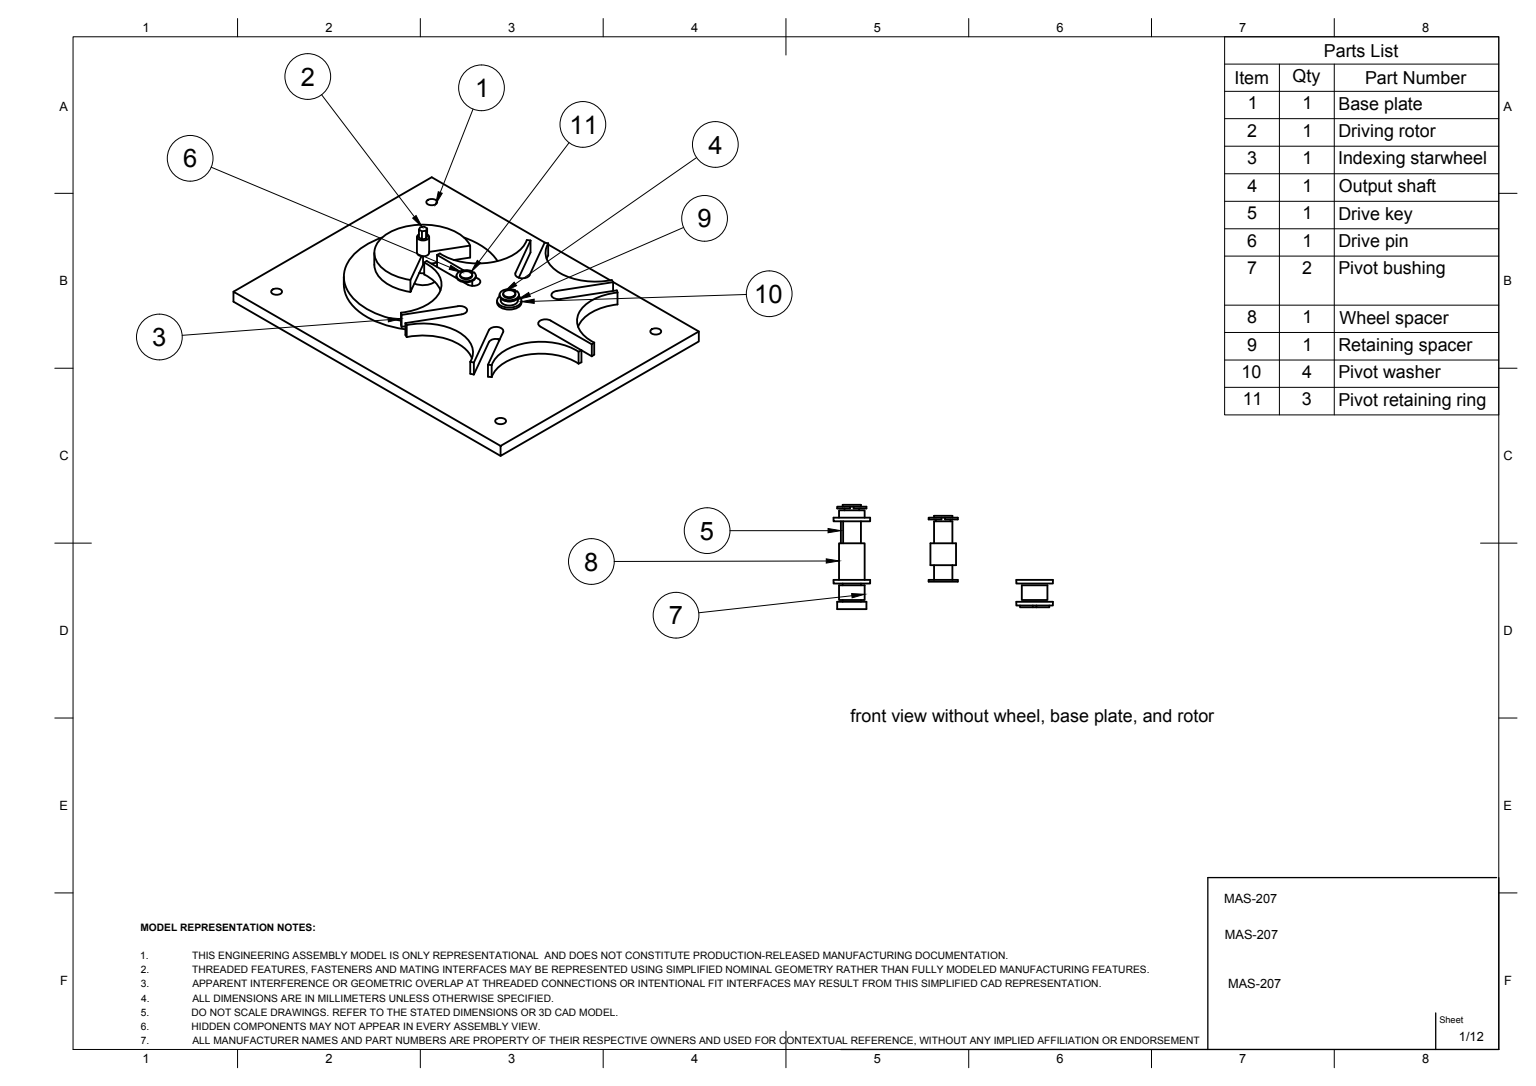
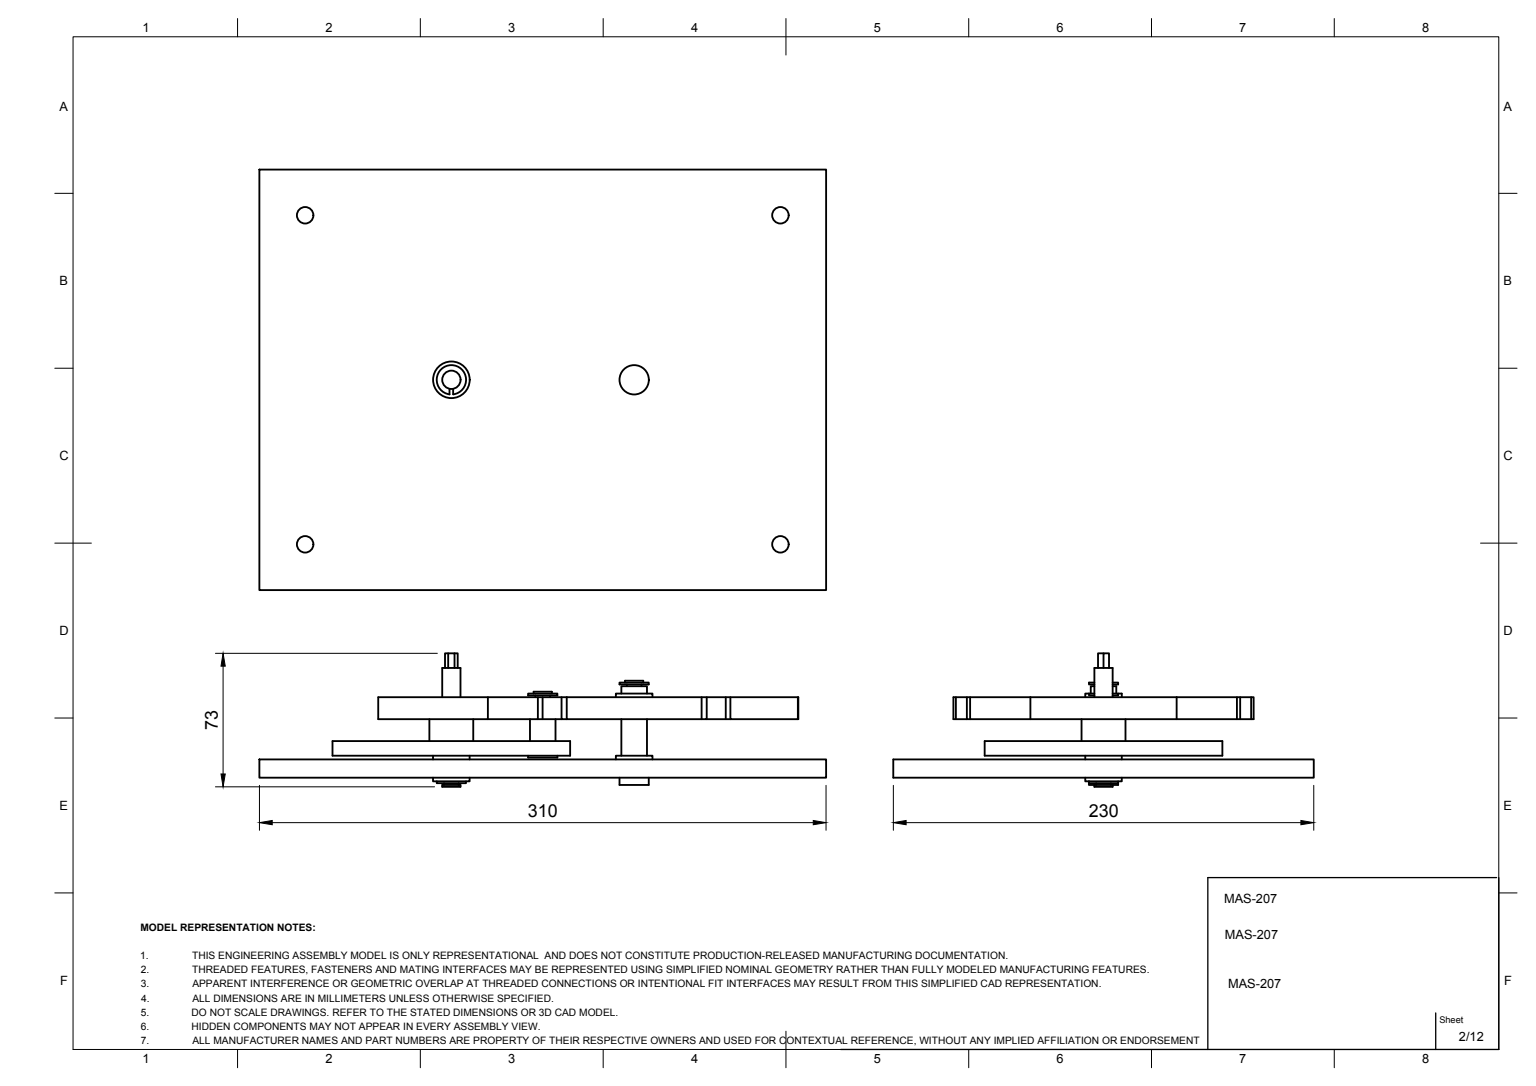
ISO-10303-21;
HEADER;
/* Generated by software containing ST-Developer
 * from STEP Tools, Inc. (www.steptools.com) 
 */

FILE_DESCRIPTION(
/* description */ ('Independent six-slot Geneva indexer. Center distance100, drive radius
50, 60degree indexing per input revolution with120degree engagement an
d240degree dwell. Native machined concave locking faces and relieved d
isk; replaceable retained drive pin; keyed output shaft. Geometry traj
ectory checks use calculated indexing positions, not a contact-dynamic
s simulation. No load or production rating assigned.'),
/* implementation_level */ '2;1');

FILE_NAME(
/* name */ 'MAS-207.step',
/* time_stamp */ '2026-11-09T17:53:22-08:00',
/* author */ (''),
/* organization */ (''),
/* preprocessor_version */ 'ST-DEVELOPER v20.2',
/* originating_system */ 'Autodesk Translation Framework v15.17.0.0',
/* authorisation */ '');

FILE_SCHEMA (('AUTOMOTIVE_DESIGN { 1 0 10303 214 3 1 1 }'));
ENDSEC;

DATA;
#10=MECHANICAL_DESIGN_GEOMETRIC_PRESENTATION_REPRESENTATION('',(#101,#102,
#103,#104,#105,#106,#107,#108,#109,#110,#111),#4149);
#11=ITEM_DEFINED_TRANSFORMATION($,$,#2429,#2700);
#12=ITEM_DEFINED_TRANSFORMATION($,$,#2454,#2701);
#13=ITEM_DEFINED_TRANSFORMATION($,$,#2502,#2702);
#14=ITEM_DEFINED_TRANSFORMATION($,$,#2595,#2703);
#15=ITEM_DEFINED_TRANSFORMATION($,$,#2620,#2704);
#16=ITEM_DEFINED_TRANSFORMATION($,$,#2627,#2705);
#17=ITEM_DEFINED_TRANSFORMATION($,$,#2653,#2706);
#18=ITEM_DEFINED_TRANSFORMATION($,$,#2653,#2707);
#19=ITEM_DEFINED_TRANSFORMATION($,$,#2662,#2708);
#20=ITEM_DEFINED_TRANSFORMATION($,$,#2671,#2709);
#21=ITEM_DEFINED_TRANSFORMATION($,$,#2680,#2710);
#22=ITEM_DEFINED_TRANSFORMATION($,$,#2680,#2711);
#23=ITEM_DEFINED_TRANSFORMATION($,$,#2680,#2712);
#24=ITEM_DEFINED_TRANSFORMATION($,$,#2680,#2713);
#25=ITEM_DEFINED_TRANSFORMATION($,$,#2689,#2714);
#26=ITEM_DEFINED_TRANSFORMATION($,$,#2689,#2715);
#27=ITEM_DEFINED_TRANSFORMATION($,$,#2689,#2716);
#28=(
REPRESENTATION_RELATIONSHIP($,$,#4196,#4195)
REPRESENTATION_RELATIONSHIP_WITH_TRANSFORMATION(#11)
SHAPE_REPRESENTATION_RELATIONSHIP()
);
#29=(
REPRESENTATION_RELATIONSHIP($,$,#4197,#4195)
REPRESENTATION_RELATIONSHIP_WITH_TRANSFORMATION(#12)
SHAPE_REPRESENTATION_RELATIONSHIP()
);
#30=(
REPRESENTATION_RELATIONSHIP($,$,#4198,#4195)
REPRESENTATION_RELATIONSHIP_WITH_TRANSFORMATION(#13)
SHAPE_REPRESENTATION_RELATIONSHIP()
);
#31=(
REPRESENTATION_RELATIONSHIP($,$,#4199,#4195)
REPRESENTATION_RELATIONSHIP_WITH_TRANSFORMATION(#14)
SHAPE_REPRESENTATION_RELATIONSHIP()
);
#32=(
REPRESENTATION_RELATIONSHIP($,$,#4200,#4195)
REPRESENTATION_RELATIONSHIP_WITH_TRANSFORMATION(#15)
SHAPE_REPRESENTATION_RELATIONSHIP()
);
#33=(
REPRESENTATION_RELATIONSHIP($,$,#4201,#4195)
REPRESENTATION_RELATIONSHIP_WITH_TRANSFORMATION(#16)
SHAPE_REPRESENTATION_RELATIONSHIP()
);
#34=(
REPRESENTATION_RELATIONSHIP($,$,#4202,#4195)
REPRESENTATION_RELATIONSHIP_WITH_TRANSFORMATION(#17)
SHAPE_REPRESENTATION_RELATIONSHIP()
);
#35=(
REPRESENTATION_RELATIONSHIP($,$,#4202,#4195)
REPRESENTATION_RELATIONSHIP_WITH_TRANSFORMATION(#18)
SHAPE_REPRESENTATION_RELATIONSHIP()
);
#36=(
REPRESENTATION_RELATIONSHIP($,$,#4203,#4195)
REPRESENTATION_RELATIONSHIP_WITH_TRANSFORMATION(#19)
SHAPE_REPRESENTATION_RELATIONSHIP()
);
#37=(
REPRESENTATION_RELATIONSHIP($,$,#4204,#4195)
REPRESENTATION_RELATIONSHIP_WITH_TRANSFORMATION(#20)
SHAPE_REPRESENTATION_RELATIONSHIP()
);
#38=(
REPRESENTATION_RELATIONSHIP($,$,#4205,#4195)
REPRESENTATION_RELATIONSHIP_WITH_TRANSFORMATION(#21)
SHAPE_REPRESENTATION_RELATIONSHIP()
);
#39=(
REPRESENTATION_RELATIONSHIP($,$,#4205,#4195)
REPRESENTATION_RELATIONSHIP_WITH_TRANSFORMATION(#22)
SHAPE_REPRESENTATION_RELATIONSHIP()
);
#40=(
REPRESENTATION_RELATIONSHIP($,$,#4205,#4195)
REPRESENTATION_RELATIONSHIP_WITH_TRANSFORMATION(#23)
SHAPE_REPRESENTATION_RELATIONSHIP()
);
#41=(
REPRESENTATION_RELATIONSHIP($,$,#4205,#4195)
REPRESENTATION_RELATIONSHIP_WITH_TRANSFORMATION(#24)
SHAPE_REPRESENTATION_RELATIONSHIP()
);
#42=(
REPRESENTATION_RELATIONSHIP($,$,#4206,#4195)
REPRESENTATION_RELATIONSHIP_WITH_TRANSFORMATION(#25)
SHAPE_REPRESENTATION_RELATIONSHIP()
);
#43=(
REPRESENTATION_RELATIONSHIP($,$,#4206,#4195)
REPRESENTATION_RELATIONSHIP_WITH_TRANSFORMATION(#26)
SHAPE_REPRESENTATION_RELATIONSHIP()
);
#44=(
REPRESENTATION_RELATIONSHIP($,$,#4206,#4195)
REPRESENTATION_RELATIONSHIP_WITH_TRANSFORMATION(#27)
SHAPE_REPRESENTATION_RELATIONSHIP()
);
#45=CONTEXT_DEPENDENT_SHAPE_REPRESENTATION(#28,#4178);
#46=CONTEXT_DEPENDENT_SHAPE_REPRESENTATION(#29,#4179);
#47=CONTEXT_DEPENDENT_SHAPE_REPRESENTATION(#30,#4180);
#48=CONTEXT_DEPENDENT_SHAPE_REPRESENTATION(#31,#4181);
#49=CONTEXT_DEPENDENT_SHAPE_REPRESENTATION(#32,#4182);
#50=CONTEXT_DEPENDENT_SHAPE_REPRESENTATION(#33,#4183);
#51=CONTEXT_DEPENDENT_SHAPE_REPRESENTATION(#34,#4184);
#52=CONTEXT_DEPENDENT_SHAPE_REPRESENTATION(#35,#4185);
#53=CONTEXT_DEPENDENT_SHAPE_REPRESENTATION(#36,#4186);
#54=CONTEXT_DEPENDENT_SHAPE_REPRESENTATION(#37,#4187);
#55=CONTEXT_DEPENDENT_SHAPE_REPRESENTATION(#38,#4188);
#56=CONTEXT_DEPENDENT_SHAPE_REPRESENTATION(#39,#4189);
#57=CONTEXT_DEPENDENT_SHAPE_REPRESENTATION(#40,#4190);
#58=CONTEXT_DEPENDENT_SHAPE_REPRESENTATION(#41,#4191);
#59=CONTEXT_DEPENDENT_SHAPE_REPRESENTATION(#42,#4192);
#60=CONTEXT_DEPENDENT_SHAPE_REPRESENTATION(#43,#4193);
#61=CONTEXT_DEPENDENT_SHAPE_REPRESENTATION(#44,#4194);
#62=NEXT_ASSEMBLY_USAGE_OCCURRENCE('Base plate:1','Base plate:1',
'Base plate:1',#4208,#4209,'Base plate:1');
#63=NEXT_ASSEMBLY_USAGE_OCCURRENCE('Driving rotor:1','Driving rotor:1',
'Driving rotor:1',#4208,#4210,'Driving rotor:1');
#64=NEXT_ASSEMBLY_USAGE_OCCURRENCE('Indexing starwheel:1',
'Indexing starwheel:1','Indexing starwheel:1',#4208,#4211,
'Indexing starwheel:1');
#65=NEXT_ASSEMBLY_USAGE_OCCURRENCE('Output shaft:1','Output shaft:1',
'Output shaft:1',#4208,#4212,'Output shaft:1');
#66=NEXT_ASSEMBLY_USAGE_OCCURRENCE('Drive key:1','Drive key:1',
'Drive key:1',#4208,#4213,'Drive key:1');
#67=NEXT_ASSEMBLY_USAGE_OCCURRENCE('Drive pin:1','Drive pin:1',
'Drive pin:1',#4208,#4214,'Drive pin:1');
#68=NEXT_ASSEMBLY_USAGE_OCCURRENCE('Pivot bushing:1','Pivot bushing:1',
'Pivot bushing:1',#4208,#4215,'Pivot bushing:1');
#69=NEXT_ASSEMBLY_USAGE_OCCURRENCE('Pivot bushing:2','Pivot bushing:2',
'Pivot bushing:2',#4208,#4215,'Pivot bushing:2');
#70=NEXT_ASSEMBLY_USAGE_OCCURRENCE('Wheel spacer:1','Wheel spacer:1',
'Wheel spacer:1',#4208,#4216,'Wheel spacer:1');
#71=NEXT_ASSEMBLY_USAGE_OCCURRENCE('Retaining spacer:1',
'Retaining spacer:1','Retaining spacer:1',#4208,#4217,
'Retaining spacer:1');
#72=NEXT_ASSEMBLY_USAGE_OCCURRENCE('Pivot washer:1','Pivot washer:1',
'Pivot washer:1',#4208,#4218,'Pivot washer:1');
#73=NEXT_ASSEMBLY_USAGE_OCCURRENCE('Pivot washer:2','Pivot washer:2',
'Pivot washer:2',#4208,#4218,'Pivot washer:2');
#74=NEXT_ASSEMBLY_USAGE_OCCURRENCE('Pivot washer:3','Pivot washer:3',
'Pivot washer:3',#4208,#4218,'Pivot washer:3');
#75=NEXT_ASSEMBLY_USAGE_OCCURRENCE('Pivot washer:4','Pivot washer:4',
'Pivot washer:4',#4208,#4218,'Pivot washer:4');
#76=NEXT_ASSEMBLY_USAGE_OCCURRENCE('Pivot retaining ring:1',
'Pivot retaining ring:1','Pivot retaining ring:1',#4208,#4219,
'Pivot retaining ring:1');
#77=NEXT_ASSEMBLY_USAGE_OCCURRENCE('Pivot retaining ring:2',
'Pivot retaining ring:2','Pivot retaining ring:2',#4208,#4219,
'Pivot retaining ring:2');
#78=NEXT_ASSEMBLY_USAGE_OCCURRENCE('Pivot retaining ring:3',
'Pivot retaining ring:3','Pivot retaining ring:3',#4208,#4219,
'Pivot retaining ring:3');
#79=SHAPE_REPRESENTATION_RELATIONSHIP('SRR','None',#4196,#90);
#80=SHAPE_REPRESENTATION_RELATIONSHIP('SRR','None',#4197,#91);
#81=SHAPE_REPRESENTATION_RELATIONSHIP('SRR','None',#4198,#92);
#82=SHAPE_REPRESENTATION_RELATIONSHIP('SRR','None',#4199,#93);
#83=SHAPE_REPRESENTATION_RELATIONSHIP('SRR','None',#4200,#94);
#84=SHAPE_REPRESENTATION_RELATIONSHIP('SRR','None',#4201,#95);
#85=SHAPE_REPRESENTATION_RELATIONSHIP('SRR','None',#4202,#96);
#86=SHAPE_REPRESENTATION_RELATIONSHIP('SRR','None',#4203,#97);
#87=SHAPE_REPRESENTATION_RELATIONSHIP('SRR','None',#4204,#98);
#88=SHAPE_REPRESENTATION_RELATIONSHIP('SRR','None',#4205,#99);
#89=SHAPE_REPRESENTATION_RELATIONSHIP('SRR','None',#4206,#100);
#90=ADVANCED_BREP_SHAPE_REPRESENTATION('',(#112),#4138);
#91=ADVANCED_BREP_SHAPE_REPRESENTATION('',(#113),#4139);
#92=ADVANCED_BREP_SHAPE_REPRESENTATION('',(#114),#4140);
#93=ADVANCED_BREP_SHAPE_REPRESENTATION('',(#115),#4141);
#94=ADVANCED_BREP_SHAPE_REPRESENTATION('',(#116),#4142);
#95=ADVANCED_BREP_SHAPE_REPRESENTATION('',(#117),#4143);
#96=ADVANCED_BREP_SHAPE_REPRESENTATION('',(#118),#4144);
#97=ADVANCED_BREP_SHAPE_REPRESENTATION('',(#119),#4145);
#98=ADVANCED_BREP_SHAPE_REPRESENTATION('',(#120),#4146);
#99=ADVANCED_BREP_SHAPE_REPRESENTATION('',(#121),#4147);
#100=ADVANCED_BREP_SHAPE_REPRESENTATION('',(#122),#4148);
#101=STYLED_ITEM('',(#4260),#112);
#102=STYLED_ITEM('',(#4261),#113);
#103=STYLED_ITEM('',(#4262),#114);
#104=STYLED_ITEM('',(#4263),#115);
#105=STYLED_ITEM('',(#4264),#116);
#106=STYLED_ITEM('',(#4263),#117);
#107=STYLED_ITEM('',(#4265),#118);
#108=STYLED_ITEM('',(#4266),#119);
#109=STYLED_ITEM('',(#4266),#120);
#110=STYLED_ITEM('',(#4267),#121);
#111=STYLED_ITEM('',(#4268),#122);
#112=MANIFOLD_SOLID_BREP('Body1',#2295);
#113=MANIFOLD_SOLID_BREP('Body1',#2296);
#114=MANIFOLD_SOLID_BREP('Body1',#2297);
#115=MANIFOLD_SOLID_BREP('Body1',#2298);
#116=MANIFOLD_SOLID_BREP('Body1',#2299);
#117=MANIFOLD_SOLID_BREP('Body1',#2300);
#118=MANIFOLD_SOLID_BREP('Body1',#2301);
#119=MANIFOLD_SOLID_BREP('Body1',#2302);
#120=MANIFOLD_SOLID_BREP('Body1',#2303);
#121=MANIFOLD_SOLID_BREP('Body1',#2304);
#122=MANIFOLD_SOLID_BREP('Body1',#2305);
#123=FACE_BOUND('',#385,.T.);
#124=FACE_BOUND('',#386,.T.);
#125=FACE_BOUND('',#387,.T.);
#126=FACE_BOUND('',#388,.T.);
#127=FACE_BOUND('',#389,.T.);
#128=FACE_BOUND('',#390,.T.);
#129=FACE_BOUND('',#392,.T.);
#130=FACE_BOUND('',#393,.T.);
#131=FACE_BOUND('',#394,.T.);
#132=FACE_BOUND('',#395,.T.);
#133=FACE_BOUND('',#396,.T.);
#134=FACE_BOUND('',#397,.T.);
#135=FACE_BOUND('',#407,.T.);
#136=FACE_BOUND('',#409,.T.);
#137=FACE_BOUND('',#421,.T.);
#138=FACE_BOUND('',#422,.T.);
#139=FACE_BOUND('',#424,.T.);
#140=FACE_BOUND('',#425,.T.);
#141=FACE_BOUND('',#430,.T.);
#142=FACE_BOUND('',#437,.T.);
#143=FACE_BOUND('',#451,.T.);
#144=FACE_BOUND('',#483,.T.);
#145=FACE_BOUND('',#485,.T.);
#146=FACE_BOUND('',#488,.T.);
#147=FACE_BOUND('',#492,.T.);
#148=FACE_BOUND('',#501,.T.);
#149=FACE_BOUND('',#503,.T.);
#150=FACE_BOUND('',#508,.T.);
#151=FACE_BOUND('',#510,.T.);
#152=FACE_BOUND('',#513,.T.);
#153=FACE_BOUND('',#521,.T.);
#154=FACE_BOUND('',#523,.T.);
#155=FACE_BOUND('',#527,.T.);
#156=FACE_BOUND('',#529,.T.);
#157=FACE_BOUND('',#533,.T.);
#158=FACE_BOUND('',#535,.T.);
#159=FACE_BOUND('',#539,.T.);
#160=FACE_BOUND('',#541,.T.);
#161=PLANE('',#2448);
#162=PLANE('',#2449);
#163=PLANE('',#2450);
#164=PLANE('',#2451);
#165=PLANE('',#2452);
#166=PLANE('',#2453);
#167=PLANE('',#2455);
#168=PLANE('',#2456);
#169=PLANE('',#2457);
#170=PLANE('',#2458);
#171=PLANE('',#2459);
#172=PLANE('',#2460);
#173=PLANE('',#2461);
#174=PLANE('',#2465);
#175=PLANE('',#2467);
#176=PLANE('',#2474);
#177=PLANE('',#2476);
#178=PLANE('',#2478);
#179=PLANE('',#2479);
#180=PLANE('',#2480);
#181=PLANE('',#2484);
#182=PLANE('',#2491);
#183=PLANE('',#2493);
#184=PLANE('',#2500);
#185=PLANE('',#2501);
#186=PLANE('',#2503);
#187=PLANE('',#2504);
#188=PLANE('',#2505);
#189=PLANE('',#2509);
#190=PLANE('',#2558);
#191=PLANE('',#2573);
#192=PLANE('',#2574);
#193=PLANE('',#2576);
#194=PLANE('',#2577);
#195=PLANE('',#2579);
#196=PLANE('',#2580);
#197=PLANE('',#2584);
#198=PLANE('',#2585);
#199=PLANE('',#2587);
#200=PLANE('',#2588);
#201=PLANE('',#2592);
#202=PLANE('',#2593);
#203=PLANE('',#2596);
#204=PLANE('',#2597);
#205=PLANE('',#2599);
#206=PLANE('',#2600);
#207=PLANE('',#2601);
#208=PLANE('',#2606);
#209=PLANE('',#2608);
#210=PLANE('',#2612);
#211=PLANE('',#2617);
#212=PLANE('',#2619);
#213=PLANE('',#2621);
#214=PLANE('',#2622);
#215=PLANE('',#2623);
#216=PLANE('',#2624);
#217=PLANE('',#2625);
#218=PLANE('',#2626);
#219=PLANE('',#2628);
#220=PLANE('',#2631);
#221=PLANE('',#2640);
#222=PLANE('',#2642);
#223=PLANE('',#2646);
#224=PLANE('',#2650);
#225=PLANE('',#2652);
#226=PLANE('',#2660);
#227=PLANE('',#2661);
#228=PLANE('',#2669);
#229=PLANE('',#2670);
#230=PLANE('',#2678);
#231=PLANE('',#2679);
#232=PLANE('',#2687);
#233=PLANE('',#2688);
#234=PLANE('',#2690);
#235=PLANE('',#2691);
#236=PLANE('',#2692);
#237=PLANE('',#2699);
#238=FACE_OUTER_BOUND('',#374,.T.);
#239=FACE_OUTER_BOUND('',#375,.T.);
#240=FACE_OUTER_BOUND('',#376,.T.);
#241=FACE_OUTER_BOUND('',#377,.T.);
#242=FACE_OUTER_BOUND('',#378,.T.);
#243=FACE_OUTER_BOUND('',#379,.T.);
#244=FACE_OUTER_BOUND('',#380,.T.);
#245=FACE_OUTER_BOUND('',#381,.T.);
#246=FACE_OUTER_BOUND('',#382,.T.);
#247=FACE_OUTER_BOUND('',#383,.T.);
#248=FACE_OUTER_BOUND('',#384,.T.);
#249=FACE_OUTER_BOUND('',#391,.T.);
#250=FACE_OUTER_BOUND('',#398,.T.);
#251=FACE_OUTER_BOUND('',#399,.T.);
#252=FACE_OUTER_BOUND('',#400,.T.);
#253=FACE_OUTER_BOUND('',#401,.T.);
#254=FACE_OUTER_BOUND('',#402,.T.);
#255=FACE_OUTER_BOUND('',#403,.T.);
#256=FACE_OUTER_BOUND('',#404,.T.);
#257=FACE_OUTER_BOUND('',#405,.T.);
#258=FACE_OUTER_BOUND('',#406,.T.);
#259=FACE_OUTER_BOUND('',#408,.T.);
#260=FACE_OUTER_BOUND('',#410,.T.);
#261=FACE_OUTER_BOUND('',#411,.T.);
#262=FACE_OUTER_BOUND('',#412,.T.);
#263=FACE_OUTER_BOUND('',#413,.T.);
#264=FACE_OUTER_BOUND('',#414,.T.);
#265=FACE_OUTER_BOUND('',#415,.T.);
#266=FACE_OUTER_BOUND('',#416,.T.);
#267=FACE_OUTER_BOUND('',#417,.T.);
#268=FACE_OUTER_BOUND('',#418,.T.);
#269=FACE_OUTER_BOUND('',#419,.T.);
#270=FACE_OUTER_BOUND('',#420,.T.);
#271=FACE_OUTER_BOUND('',#423,.T.);
#272=FACE_OUTER_BOUND('',#426,.T.);
#273=FACE_OUTER_BOUND('',#427,.T.);
#274=FACE_OUTER_BOUND('',#428,.T.);
#275=FACE_OUTER_BOUND('',#429,.T.);
#276=FACE_OUTER_BOUND('',#431,.T.);
#277=FACE_OUTER_BOUND('',#432,.T.);
#278=FACE_OUTER_BOUND('',#433,.T.);
#279=FACE_OUTER_BOUND('',#434,.T.);
#280=FACE_OUTER_BOUND('',#435,.T.);
#281=FACE_OUTER_BOUND('',#436,.T.);
#282=FACE_OUTER_BOUND('',#438,.T.);
#283=FACE_OUTER_BOUND('',#439,.T.);
#284=FACE_OUTER_BOUND('',#440,.T.);
#285=FACE_OUTER_BOUND('',#441,.T.);
#286=FACE_OUTER_BOUND('',#442,.T.);
#287=FACE_OUTER_BOUND('',#443,.T.);
#288=FACE_OUTER_BOUND('',#444,.T.);
#289=FACE_OUTER_BOUND('',#445,.T.);
#290=FACE_OUTER_BOUND('',#446,.T.);
#291=FACE_OUTER_BOUND('',#447,.T.);
#292=FACE_OUTER_BOUND('',#448,.T.);
#293=FACE_OUTER_BOUND('',#449,.T.);
#294=FACE_OUTER_BOUND('',#450,.T.);
#295=FACE_OUTER_BOUND('',#452,.T.);
#296=FACE_OUTER_BOUND('',#453,.T.);
#297=FACE_OUTER_BOUND('',#454,.T.);
#298=FACE_OUTER_BOUND('',#455,.T.);
#299=FACE_OUTER_BOUND('',#456,.T.);
#300=FACE_OUTER_BOUND('',#457,.T.);
#301=FACE_OUTER_BOUND('',#458,.T.);
#302=FACE_OUTER_BOUND('',#459,.T.);
#303=FACE_OUTER_BOUND('',#460,.T.);
#304=FACE_OUTER_BOUND('',#461,.T.);
#305=FACE_OUTER_BOUND('',#462,.T.);
#306=FACE_OUTER_BOUND('',#463,.T.);
#307=FACE_OUTER_BOUND('',#464,.T.);
#308=FACE_OUTER_BOUND('',#465,.T.);
#309=FACE_OUTER_BOUND('',#466,.T.);
#310=FACE_OUTER_BOUND('',#467,.T.);
#311=FACE_OUTER_BOUND('',#468,.T.);
#312=FACE_OUTER_BOUND('',#469,.T.);
#313=FACE_OUTER_BOUND('',#470,.T.);
#314=FACE_OUTER_BOUND('',#471,.T.);
#315=FACE_OUTER_BOUND('',#472,.T.);
#316=FACE_OUTER_BOUND('',#473,.T.);
#317=FACE_OUTER_BOUND('',#474,.T.);
#318=FACE_OUTER_BOUND('',#475,.T.);
#319=FACE_OUTER_BOUND('',#476,.T.);
#320=FACE_OUTER_BOUND('',#477,.T.);
#321=FACE_OUTER_BOUND('',#478,.T.);
#322=FACE_OUTER_BOUND('',#479,.T.);
#323=FACE_OUTER_BOUND('',#480,.T.);
#324=FACE_OUTER_BOUND('',#481,.T.);
#325=FACE_OUTER_BOUND('',#482,.T.);
#326=FACE_OUTER_BOUND('',#484,.T.);
#327=FACE_OUTER_BOUND('',#486,.T.);
#328=FACE_OUTER_BOUND('',#487,.T.);
#329=FACE_OUTER_BOUND('',#489,.T.);
#330=FACE_OUTER_BOUND('',#490,.T.);
#331=FACE_OUTER_BOUND('',#491,.T.);
#332=FACE_OUTER_BOUND('',#493,.T.);
#333=FACE_OUTER_BOUND('',#494,.T.);
#334=FACE_OUTER_BOUND('',#495,.T.);
#335=FACE_OUTER_BOUND('',#496,.T.);
#336=FACE_OUTER_BOUND('',#497,.T.);
#337=FACE_OUTER_BOUND('',#498,.T.);
#338=FACE_OUTER_BOUND('',#499,.T.);
#339=FACE_OUTER_BOUND('',#500,.T.);
#340=FACE_OUTER_BOUND('',#502,.T.);
#341=FACE_OUTER_BOUND('',#504,.T.);
#342=FACE_OUTER_BOUND('',#505,.T.);
#343=FACE_OUTER_BOUND('',#506,.T.);
#344=FACE_OUTER_BOUND('',#507,.T.);
#345=FACE_OUTER_BOUND('',#509,.T.);
#346=FACE_OUTER_BOUND('',#511,.T.);
#347=FACE_OUTER_BOUND('',#512,.T.);
#348=FACE_OUTER_BOUND('',#514,.T.);
#349=FACE_OUTER_BOUND('',#515,.T.);
#350=FACE_OUTER_BOUND('',#516,.T.);
#351=FACE_OUTER_BOUND('',#517,.T.);
#352=FACE_OUTER_BOUND('',#518,.T.);
#353=FACE_OUTER_BOUND('',#519,.T.);
#354=FACE_OUTER_BOUND('',#520,.T.);
#355=FACE_OUTER_BOUND('',#522,.T.);
#356=FACE_OUTER_BOUND('',#524,.T.);
#357=FACE_OUTER_BOUND('',#525,.T.);
#358=FACE_OUTER_BOUND('',#526,.T.);
#359=FACE_OUTER_BOUND('',#528,.T.);
#360=FACE_OUTER_BOUND('',#530,.T.);
#361=FACE_OUTER_BOUND('',#531,.T.);
#362=FACE_OUTER_BOUND('',#532,.T.);
#363=FACE_OUTER_BOUND('',#534,.T.);
#364=FACE_OUTER_BOUND('',#536,.T.);
#365=FACE_OUTER_BOUND('',#537,.T.);
#366=FACE_OUTER_BOUND('',#538,.T.);
#367=FACE_OUTER_BOUND('',#540,.T.);
#368=FACE_OUTER_BOUND('',#542,.T.);
#369=FACE_OUTER_BOUND('',#543,.T.);
#370=FACE_OUTER_BOUND('',#544,.T.);
#371=FACE_OUTER_BOUND('',#545,.T.);
#372=FACE_OUTER_BOUND('',#546,.T.);
#373=FACE_OUTER_BOUND('',#547,.T.);
#374=EDGE_LOOP('',(#1508,#1509,#1510,#1511));
#375=EDGE_LOOP('',(#1512,#1513,#1514,#1515));
#376=EDGE_LOOP('',(#1516,#1517,#1518,#1519));
#377=EDGE_LOOP('',(#1520,#1521,#1522,#1523));
#378=EDGE_LOOP('',(#1524,#1525,#1526,#1527));
#379=EDGE_LOOP('',(#1528,#1529,#1530,#1531));
#380=EDGE_LOOP('',(#1532,#1533,#1534,#1535));
#381=EDGE_LOOP('',(#1536,#1537,#1538,#1539));
#382=EDGE_LOOP('',(#1540,#1541,#1542,#1543));
#383=EDGE_LOOP('',(#1544,#1545,#1546,#1547));
#384=EDGE_LOOP('',(#1548,#1549,#1550,#1551));
#385=EDGE_LOOP('',(#1552));
#386=EDGE_LOOP('',(#1553));
#387=EDGE_LOOP('',(#1554));
#388=EDGE_LOOP('',(#1555));
#389=EDGE_LOOP('',(#1556));
#390=EDGE_LOOP('',(#1557));
#391=EDGE_LOOP('',(#1558,#1559,#1560,#1561));
#392=EDGE_LOOP('',(#1562));
#393=EDGE_LOOP('',(#1563));
#394=EDGE_LOOP('',(#1564));
#395=EDGE_LOOP('',(#1565));
#396=EDGE_LOOP('',(#1566));
#397=EDGE_LOOP('',(#1567));
#398=EDGE_LOOP('',(#1568,#1569,#1570,#1571));
#399=EDGE_LOOP('',(#1572,#1573,#1574,#1575));
#400=EDGE_LOOP('',(#1576,#1577,#1578,#1579));
#401=EDGE_LOOP('',(#1580,#1581,#1582,#1583));
#402=EDGE_LOOP('',(#1584,#1585,#1586,#1587));
#403=EDGE_LOOP('',(#1588,#1589,#1590,#1591));
#404=EDGE_LOOP('',(#1592,#1593,#1594,#1595,#1596,#1597));
#405=EDGE_LOOP('',(#1598,#1599,#1600,#1601));
#406=EDGE_LOOP('',(#1602));
#407=EDGE_LOOP('',(#1603));
#408=EDGE_LOOP('',(#1604));
#409=EDGE_LOOP('',(#1605));
#410=EDGE_LOOP('',(#1606,#1607,#1608,#1609));
#411=EDGE_LOOP('',(#1610,#1611,#1612,#1613));
#412=EDGE_LOOP('',(#1614,#1615,#1616));
#413=EDGE_LOOP('',(#1617,#1618,#1619));
#414=EDGE_LOOP('',(#1620,#1621,#1622,#1623,#1624,#1625));
#415=EDGE_LOOP('',(#1626,#1627,#1628,#1629,#1630,#1631));
#416=EDGE_LOOP('',(#1632,#1633,#1634,#1635,#1636));
#417=EDGE_LOOP('',(#1637,#1638,#1639,#1640,#1641));
#418=EDGE_LOOP('',(#1642,#1643,#1644,#1645));
#419=EDGE_LOOP('',(#1646,#1647,#1648,#1649,#1650,#1651));
#420=EDGE_LOOP('',(#1652));
#421=EDGE_LOOP('',(#1653));
#422=EDGE_LOOP('',(#1654));
#423=EDGE_LOOP('',(#1655));
#424=EDGE_LOOP('',(#1656));
#425=EDGE_LOOP('',(#1657));
#426=EDGE_LOOP('',(#1658,#1659,#1660,#1661));
#427=EDGE_LOOP('',(#1662,#1663,#1664,#1665));
#428=EDGE_LOOP('',(#1666,#1667,#1668,#1669,#1670,#1671));
#429=EDGE_LOOP('',(#1672));
#430=EDGE_LOOP('',(#1673,#1674,#1675,#1676,#1677,#1678));
#431=EDGE_LOOP('',(#1679));
#432=EDGE_LOOP('',(#1680,#1681,#1682,#1683));
#433=EDGE_LOOP('',(#1684,#1685,#1686,#1687));
#434=EDGE_LOOP('',(#1688,#1689,#1690,#1691));
#435=EDGE_LOOP('',(#1692,#1693,#1694,#1695));
#436=EDGE_LOOP('',(#1696,#1697,#1698,#1699,#1700,#1701,#1702,#1703,#1704,
#1705,#1706,#1707,#1708,#1709,#1710,#1711,#1712,#1713,#1714,#1715,#1716,
#1717,#1718,#1719,#1720,#1721,#1722,#1723,#1724,#1725,#1726,#1727,#1728,
#1729,#1730,#1731));
#437=EDGE_LOOP('',(#1732,#1733,#1734,#1735));
#438=EDGE_LOOP('',(#1736,#1737,#1738,#1739));
#439=EDGE_LOOP('',(#1740,#1741,#1742,#1743));
#440=EDGE_LOOP('',(#1744,#1745,#1746,#1747));
#441=EDGE_LOOP('',(#1748,#1749,#1750,#1751));
#442=EDGE_LOOP('',(#1752,#1753,#1754,#1755));
#443=EDGE_LOOP('',(#1756,#1757,#1758,#1759));
#444=EDGE_LOOP('',(#1760,#1761,#1762,#1763));
#445=EDGE_LOOP('',(#1764,#1765,#1766,#1767));
#446=EDGE_LOOP('',(#1768,#1769,#1770,#1771));
#447=EDGE_LOOP('',(#1772,#1773,#1774,#1775));
#448=EDGE_LOOP('',(#1776,#1777,#1778,#1779));
#449=EDGE_LOOP('',(#1780,#1781,#1782,#1783));
#450=EDGE_LOOP('',(#1784,#1785,#1786,#1787,#1788,#1789,#1790,#1791,#1792,
#1793,#1794,#1795,#1796,#1797,#1798,#1799,#1800,#1801,#1802,#1803,#1804,
#1805,#1806,#1807,#1808,#1809,#1810,#1811,#1812,#1813,#1814,#1815,#1816,
#1817,#1818,#1819));
#451=EDGE_LOOP('',(#1820,#1821,#1822,#1823));
#452=EDGE_LOOP('',(#1824,#1825,#1826,#1827));
#453=EDGE_LOOP('',(#1828,#1829,#1830,#1831));
#454=EDGE_LOOP('',(#1832,#1833,#1834,#1835));
#455=EDGE_LOOP('',(#1836,#1837,#1838,#1839));
#456=EDGE_LOOP('',(#1840,#1841,#1842,#1843));
#457=EDGE_LOOP('',(#1844,#1845,#1846,#1847));
#458=EDGE_LOOP('',(#1848,#1849,#1850,#1851));
#459=EDGE_LOOP('',(#1852,#1853,#1854,#1855));
#460=EDGE_LOOP('',(#1856,#1857,#1858,#1859));
#461=EDGE_LOOP('',(#1860,#1861,#1862,#1863));
#462=EDGE_LOOP('',(#1864,#1865,#1866,#1867));
#463=EDGE_LOOP('',(#1868,#1869,#1870,#1871));
#464=EDGE_LOOP('',(#1872,#1873,#1874,#1875));
#465=EDGE_LOOP('',(#1876,#1877,#1878,#1879));
#466=EDGE_LOOP('',(#1880,#1881,#1882,#1883));
#467=EDGE_LOOP('',(#1884,#1885,#1886,#1887));
#468=EDGE_LOOP('',(#1888,#1889,#1890,#1891));
#469=EDGE_LOOP('',(#1892,#1893,#1894,#1895));
#470=EDGE_LOOP('',(#1896,#1897,#1898,#1899));
#471=EDGE_LOOP('',(#1900,#1901,#1902,#1903));
#472=EDGE_LOOP('',(#1904,#1905,#1906,#1907));
#473=EDGE_LOOP('',(#1908,#1909,#1910,#1911));
#474=EDGE_LOOP('',(#1912,#1913,#1914,#1915));
#475=EDGE_LOOP('',(#1916,#1917,#1918,#1919));
#476=EDGE_LOOP('',(#1920,#1921,#1922,#1923));
#477=EDGE_LOOP('',(#1924,#1925,#1926,#1927));
#478=EDGE_LOOP('',(#1928,#1929,#1930,#1931));
#479=EDGE_LOOP('',(#1932,#1933,#1934,#1935));
#480=EDGE_LOOP('',(#1936,#1937,#1938,#1939));
#481=EDGE_LOOP('',(#1940,#1941,#1942,#1943));
#482=EDGE_LOOP('',(#1944));
#483=EDGE_LOOP('',(#1945));
#484=EDGE_LOOP('',(#1946));
#485=EDGE_LOOP('',(#1947));
#486=EDGE_LOOP('',(#1948,#1949,#1950,#1951));
#487=EDGE_LOOP('',(#1952));
#488=EDGE_LOOP('',(#1953));
#489=EDGE_LOOP('',(#1954,#1955,#1956,#1957));
#490=EDGE_LOOP('',(#1958));
#491=EDGE_LOOP('',(#1959,#1960,#1961,#1962));
#492=EDGE_LOOP('',(#1963,#1964,#1965,#1966));
#493=EDGE_LOOP('',(#1967));
#494=EDGE_LOOP('',(#1968,#1969,#1970,#1971));
#495=EDGE_LOOP('',(#1972,#1973,#1974,#1975));
#496=EDGE_LOOP('',(#1976,#1977,#1978,#1979));
#497=EDGE_LOOP('',(#1980,#1981,#1982,#1983));
#498=EDGE_LOOP('',(#1984,#1985,#1986,#1987));
#499=EDGE_LOOP('',(#1988,#1989,#1990,#1991));
#500=EDGE_LOOP('',(#1992));
#501=EDGE_LOOP('',(#1993));
#502=EDGE_LOOP('',(#1994));
#503=EDGE_LOOP('',(#1995));
#504=EDGE_LOOP('',(#1996,#1997,#1998,#1999));
#505=EDGE_LOOP('',(#2000,#2001,#2002,#2003));
#506=EDGE_LOOP('',(#2004,#2005,#2006,#2007));
#507=EDGE_LOOP('',(#2008));
#508=EDGE_LOOP('',(#2009));
#509=EDGE_LOOP('',(#2010));
#510=EDGE_LOOP('',(#2011));
#511=EDGE_LOOP('',(#2012,#2013,#2014,#2015));
#512=EDGE_LOOP('',(#2016));
#513=EDGE_LOOP('',(#2017));
#514=EDGE_LOOP('',(#2018,#2019,#2020,#2021));
#515=EDGE_LOOP('',(#2022));
#516=EDGE_LOOP('',(#2023,#2024,#2025,#2026));
#517=EDGE_LOOP('',(#2027));
#518=EDGE_LOOP('',(#2028,#2029,#2030,#2031));
#519=EDGE_LOOP('',(#2032,#2033,#2034,#2035));
#520=EDGE_LOOP('',(#2036));
#521=EDGE_LOOP('',(#2037));
#522=EDGE_LOOP('',(#2038));
#523=EDGE_LOOP('',(#2039));
#524=EDGE_LOOP('',(#2040,#2041,#2042,#2043));
#525=EDGE_LOOP('',(#2044,#2045,#2046,#2047));
#526=EDGE_LOOP('',(#2048));
#527=EDGE_LOOP('',(#2049));
#528=EDGE_LOOP('',(#2050));
#529=EDGE_LOOP('',(#2051));
#530=EDGE_LOOP('',(#2052,#2053,#2054,#2055));
#531=EDGE_LOOP('',(#2056,#2057,#2058,#2059));
#532=EDGE_LOOP('',(#2060));
#533=EDGE_LOOP('',(#2061));
#534=EDGE_LOOP('',(#2062));
#535=EDGE_LOOP('',(#2063));
#536=EDGE_LOOP('',(#2064,#2065,#2066,#2067));
#537=EDGE_LOOP('',(#2068,#2069,#2070,#2071));
#538=EDGE_LOOP('',(#2072));
#539=EDGE_LOOP('',(#2073));
#540=EDGE_LOOP('',(#2074));
#541=EDGE_LOOP('',(#2075));
#542=EDGE_LOOP('',(#2076,#2077,#2078,#2079));
#543=EDGE_LOOP('',(#2080,#2081,#2082,#2083));
#544=EDGE_LOOP('',(#2084,#2085,#2086,#2087));
#545=EDGE_LOOP('',(#2088,#2089,#2090,#2091));
#546=EDGE_LOOP('',(#2092,#2093,#2094,#2095));
#547=EDGE_LOOP('',(#2096,#2097,#2098,#2099));
#548=LINE('',#3473,#720);
#549=LINE('',#3479,#721);
#550=LINE('',#3485,#722);
#551=LINE('',#3491,#723);
#552=LINE('',#3497,#724);
#553=LINE('',#3503,#725);
#554=LINE('',#3508,#726);
#555=LINE('',#3510,#727);
#556=LINE('',#3512,#728);
#557=LINE('',#3513,#729);
#558=LINE('',#3516,#730);
#559=LINE('',#3518,#731);
#560=LINE('',#3519,#732);
#561=LINE('',#3522,#733);
#562=LINE('',#3524,#734);
#563=LINE('',#3525,#735);
#564=LINE('',#3527,#736);
#565=LINE('',#3528,#737);
#566=LINE('',#3535,#738);
#567=LINE('',#3537,#739);
#568=LINE('',#3539,#740);
#569=LINE('',#3540,#741);
#570=LINE('',#3543,#742);
#571=LINE('',#3545,#743);
#572=LINE('',#3546,#744);
#573=LINE('',#3549,#745);
#574=LINE('',#3551,#746);
#575=LINE('',#3552,#747);
#576=LINE('',#3555,#748);
#577=LINE('',#3557,#749);
#578=LINE('',#3558,#750);
#579=LINE('',#3561,#751);
#580=LINE('',#3563,#752);
#581=LINE('',#3564,#753);
#582=LINE('',#3566,#754);
#583=LINE('',#3567,#755);
#584=LINE('',#3573,#756);
#585=LINE('',#3584,#757);
#586=LINE('',#3589,#758);
#587=LINE('',#3596,#759);
#588=LINE('',#3597,#760);
#589=LINE('',#3603,#761);
#590=LINE('',#3604,#762);
#591=LINE('',#3608,#763);
#592=LINE('',#3609,#764);
#593=LINE('',#3610,#765);
#594=LINE('',#3611,#766);
#595=LINE('',#3615,#767);
#596=LINE('',#3616,#768);
#597=LINE('',#3617,#769);
#598=LINE('',#3631,#770);
#599=LINE('',#3640,#771);
#600=LINE('',#3643,#772);
#601=LINE('',#3648,#773);
#602=LINE('',#3655,#774);
#603=LINE('',#3657,#775);
#604=LINE('',#3659,#776);
#605=LINE('',#3660,#777);
#606=LINE('',#3664,#778);
#607=LINE('',#3666,#779);
#608=LINE('',#3668,#780);
#609=LINE('',#3669,#781);
#610=LINE('',#3671,#782);
#611=LINE('',#3672,#783);
#612=LINE('',#3683,#784);
#613=LINE('',#3687,#785);
#614=LINE('',#3695,#786);
#615=LINE('',#3699,#787);
#616=LINE('',#3707,#788);
#617=LINE('',#3711,#789);
#618=LINE('',#3719,#790);
#619=LINE('',#3723,#791);
#620=LINE('',#3731,#792);
#621=LINE('',#3735,#793);
#622=LINE('',#3743,#794);
#623=LINE('',#3747,#795);
#624=LINE('',#3751,#796);
#625=LINE('',#3753,#797);
#626=LINE('',#3757,#798);
#627=LINE('',#3759,#799);
#628=LINE('',#3763,#800);
#629=LINE('',#3765,#801);
#630=LINE('',#3769,#802);
#631=LINE('',#3771,#803);
#632=LINE('',#3775,#804);
#633=LINE('',#3777,#805);
#634=LINE('',#3781,#806);
#635=LINE('',#3784,#807);
#636=LINE('',#3787,#808);
#637=LINE('',#3792,#809);
#638=LINE('',#3795,#810);
#639=LINE('',#3799,#811);
#640=LINE('',#3803,#812);
#641=LINE('',#3807,#813);
#642=LINE('',#3811,#814);
#643=LINE('',#3815,#815);
#644=LINE('',#3818,#816);
#645=LINE('',#3822,#817);
#646=LINE('',#3825,#818);
#647=LINE('',#3829,#819);
#648=LINE('',#3832,#820);
#649=LINE('',#3836,#821);
#650=LINE('',#3839,#822);
#651=LINE('',#3843,#823);
#652=LINE('',#3848,#824);
#653=LINE('',#3851,#825);
#654=LINE('',#3853,#826);
#655=LINE('',#3855,#827);
#656=LINE('',#3857,#828);
#657=LINE('',#3859,#829);
#658=LINE('',#3862,#830);
#659=LINE('',#3863,#831);
#660=LINE('',#3865,#832);
#661=LINE('',#3868,#833);
#662=LINE('',#3869,#834);
#663=LINE('',#3871,#835);
#664=LINE('',#3876,#836);
#665=LINE('',#3877,#837);
#666=LINE('',#3879,#838);
#667=LINE('',#3882,#839);
#668=LINE('',#3883,#840);
#669=LINE('',#3885,#841);
#670=LINE('',#3890,#842);
#671=LINE('',#3892,#843);
#672=LINE('',#3898,#844);
#673=LINE('',#3900,#845);
#674=LINE('',#3902,#846);
#675=LINE('',#3903,#847);
#676=LINE('',#3908,#848);
#677=LINE('',#3909,#849);
#678=LINE('',#3912,#850);
#679=LINE('',#3914,#851);
#680=LINE('',#3915,#852);
#681=LINE('',#3917,#853);
#682=LINE('',#3924,#854);
#683=LINE('',#3935,#855);
#684=LINE('',#3943,#856);
#685=LINE('',#3947,#857);
#686=LINE('',#3953,#858);
#687=LINE('',#3955,#859);
#688=LINE('',#3957,#860);
#689=LINE('',#3958,#861);
#690=LINE('',#3961,#862);
#691=LINE('',#3963,#863);
#692=LINE('',#3964,#864);
#693=LINE('',#3967,#865);
#694=LINE('',#3969,#866);
#695=LINE('',#3970,#867);
#696=LINE('',#3972,#868);
#697=LINE('',#3973,#869);
#698=LINE('',#3988,#870);
#699=LINE('',#3991,#871);
#700=LINE('',#3997,#872);
#701=LINE('',#4008,#873);
#702=LINE('',#4014,#874);
#703=LINE('',#4018,#875);
#704=LINE('',#4025,#876);
#705=LINE('',#4031,#877);
#706=LINE('',#4040,#878);
#707=LINE('',#4046,#879);
#708=LINE('',#4055,#880);
#709=LINE('',#4061,#881);
#710=LINE('',#4070,#882);
#711=LINE('',#4076,#883);
#712=LINE('',#4084,#884);
#713=LINE('',#4086,#885);
#714=LINE('',#4088,#886);
#715=LINE('',#4089,#887);
#716=LINE('',#4093,#888);
#717=LINE('',#4095,#889);
#718=LINE('',#4097,#890);
#719=LINE('',#4098,#891);
#720=VECTOR('',#2725,4.5);
#721=VECTOR('',#2732,4.5);
#722=VECTOR('',#2739,4.5);
#723=VECTOR('',#2746,4.5);
#724=VECTOR('',#2753,7.);
#725=VECTOR('',#2760,7.);
#726=VECTOR('',#2765,10.);
#727=VECTOR('',#2766,10.);
#728=VECTOR('',#2767,10.);
#729=VECTOR('',#2768,10.);
#730=VECTOR('',#2771,10.);
#731=VECTOR('',#2772,10.);
#732=VECTOR('',#2773,10.);
#733=VECTOR('',#2776,10.);
#734=VECTOR('',#2777,10.);
#735=VECTOR('',#2778,10.);
#736=VECTOR('',#2781,10.);
#737=VECTOR('',#2782,10.);
#738=VECTOR('',#2791,10.);
#739=VECTOR('',#2792,10.);
#740=VECTOR('',#2793,10.);
#741=VECTOR('',#2794,10.);
#742=VECTOR('',#2797,10.);
#743=VECTOR('',#2798,10.);
#744=VECTOR('',#2799,10.);
#745=VECTOR('',#2802,10.);
#746=VECTOR('',#2803,10.);
#747=VECTOR('',#2804,10.);
#748=VECTOR('',#2807,10.);
#749=VECTOR('',#2808,10.);
#750=VECTOR('',#2809,10.);
#751=VECTOR('',#2812,10.);
#752=VECTOR('',#2813,10.);
#753=VECTOR('',#2814,10.);
#754=VECTOR('',#2817,10.);
#755=VECTOR('',#2818,10.);
#756=VECTOR('',#2825,4.);
#757=VECTOR('',#2840,5.);
#758=VECTOR('',#2845,5.);
#759=VECTOR('',#2852,10.);
#760=VECTOR('',#2853,10.);
#761=VECTOR('',#2858,10.);
#762=VECTOR('',#2859,10.);
#763=VECTOR('',#2862,10.);
#764=VECTOR('',#2863,10.);
#765=VECTOR('',#2864,10.);
#766=VECTOR('',#2865,10.);
#767=VECTOR('',#2868,10.);
#768=VECTOR('',#2869,10.);
#769=VECTOR('',#2870,10.);
#770=VECTOR('',#2891,12.);
#771=VECTOR('',#2904,60.);
#772=VECTOR('',#2907,5.);
#773=VECTOR('',#2914,5.);
#774=VECTOR('',#2923,10.);
#775=VECTOR('',#2924,10.);
#776=VECTOR('',#2925,10.);
#777=VECTOR('',#2926,10.);
#778=VECTOR('',#2929,10.);
#779=VECTOR('',#2930,10.);
#780=VECTOR('',#2931,10.);
#781=VECTOR('',#2932,10.);
#782=VECTOR('',#2935,10.);
#783=VECTOR('',#2936,10.);
#784=VECTOR('',#2949,10.);
#785=VECTOR('',#2952,10.);
#786=VECTOR('',#2959,10.);
#787=VECTOR('',#2962,10.);
#788=VECTOR('',#2969,10.);
#789=VECTOR('',#2972,10.);
#790=VECTOR('',#2979,10.);
#791=VECTOR('',#2982,10.);
#792=VECTOR('',#2989,10.);
#793=VECTOR('',#2992,10.);
#794=VECTOR('',#2999,10.);
#795=VECTOR('',#3002,10.);
#796=VECTOR('',#3007,10.);
#797=VECTOR('',#3008,10.);
#798=VECTOR('',#3013,10.);
#799=VECTOR('',#3014,10.);
#800=VECTOR('',#3019,10.);
#801=VECTOR('',#3020,10.);
#802=VECTOR('',#3025,10.);
#803=VECTOR('',#3026,10.);
#804=VECTOR('',#3031,10.);
#805=VECTOR('',#3032,10.);
#806=VECTOR('',#3037,10.);
#807=VECTOR('',#3040,10.);
#808=VECTOR('',#3043,10.);
#809=VECTOR('',#3050,10.);
#810=VECTOR('',#3053,10.);
#811=VECTOR('',#3058,10.);
#812=VECTOR('',#3063,10.);
#813=VECTOR('',#3068,10.);
#814=VECTOR('',#3073,10.);
#815=VECTOR('',#3076,10.);
#816=VECTOR('',#3079,10.);
#817=VECTOR('',#3082,10.);
#818=VECTOR('',#3085,10.);
#819=VECTOR('',#3088,10.);
#820=VECTOR('',#3091,10.);
#821=VECTOR('',#3094,10.);
#822=VECTOR('',#3097,10.);
#823=VECTOR('',#3100,10.);
#824=VECTOR('',#3105,10.);
#825=VECTOR('',#3108,10.);
#826=VECTOR('',#3111,10.);
#827=VECTOR('',#3114,10.);
#828=VECTOR('',#3117,10.);
#829=VECTOR('',#3120,10.);
#830=VECTOR('',#3125,10.);
#831=VECTOR('',#3126,10.);
#832=VECTOR('',#3129,10.);
#833=VECTOR('',#3134,10.);
#834=VECTOR('',#3135,10.);
#835=VECTOR('',#3138,10.);
#836=VECTOR('',#3147,10.);
#837=VECTOR('',#3148,10.);
#838=VECTOR('',#3151,10.);
#839=VECTOR('',#3156,10.);
#840=VECTOR('',#3157,10.);
#841=VECTOR('',#3160,10.);
#842=VECTOR('',#3169,10.);
#843=VECTOR('',#3172,10.);
#844=VECTOR('',#3179,10.);
#845=VECTOR('',#3180,10.);
#846=VECTOR('',#3181,10.);
#847=VECTOR('',#3182,10.);
#848=VECTOR('',#3187,10.);
#849=VECTOR('',#3188,10.);
#850=VECTOR('',#3191,10.);
#851=VECTOR('',#3192,10.);
#852=VECTOR('',#3193,10.);
#853=VECTOR('',#3196,10.);
#854=VECTOR('',#3205,4.);
#855=VECTOR('',#3220,5.);
#856=VECTOR('',#3229,8.);
#857=VECTOR('',#3236,5.);
#858=VECTOR('',#3243,10.);
#859=VECTOR('',#3244,10.);
#860=VECTOR('',#3245,10.);
#861=VECTOR('',#3246,10.);
#862=VECTOR('',#3249,10.);
#863=VECTOR('',#3250,10.);
#864=VECTOR('',#3251,10.);
#865=VECTOR('',#3254,10.);
#866=VECTOR('',#3255,10.);
#867=VECTOR('',#3256,10.);
#868=VECTOR('',#3259,10.);
#869=VECTOR('',#3260,10.);
#870=VECTOR('',#3281,7.);
#871=VECTOR('',#3284,5.);
#872=VECTOR('',#3291,4.);
#873=VECTOR('',#3306,5.);
#874=VECTOR('',#3313,8.);
#875=VECTOR('',#3320,5.);
#876=VECTOR('',#3329,5.);
#877=VECTOR('',#3336,7.);
#878=VECTOR('',#3349,5.);
#879=VECTOR('',#3356,7.);
#880=VECTOR('',#3369,5.);
#881=VECTOR('',#3376,7.);
#882=VECTOR('',#3389,5.);
#883=VECTOR('',#3396,10.);
#884=VECTOR('',#3407,10.);
#885=VECTOR('',#3408,10.);
#886=VECTOR('',#3409,10.);
#887=VECTOR('',#3410,10.);
#888=VECTOR('',#3413,10.);
#889=VECTOR('',#3414,10.);
#890=VECTOR('',#3415,10.);
#891=VECTOR('',#3416,10.);
#892=CIRCLE('',#2431,4.5);
#893=CIRCLE('',#2432,4.5);
#894=CIRCLE('',#2434,4.5);
#895=CIRCLE('',#2435,4.5);
#896=CIRCLE('',#2437,4.5);
#897=CIRCLE('',#2438,4.5);
#898=CIRCLE('',#2440,4.5);
#899=CIRCLE('',#2441,4.5);
#900=CIRCLE('',#2443,7.);
#901=CIRCLE('',#2444,7.);
#902=CIRCLE('',#2446,7.);
#903=CIRCLE('',#2447,7.);
#904=CIRCLE('',#2463,4.);
#905=CIRCLE('',#2464,4.);
#906=CIRCLE('',#2466,5.);
#907=CIRCLE('',#2468,5.);
#908=CIRCLE('',#2470,5.);
#909=CIRCLE('',#2472,5.);
#910=CIRCLE('',#2473,5.);
#911=CIRCLE('',#2475,5.);
#912=CIRCLE('',#2477,12.);
#913=CIRCLE('',#2481,5.);
#914=CIRCLE('',#2482,5.);
#915=CIRCLE('',#2483,40.);
#916=CIRCLE('',#2485,40.);
#917=CIRCLE('',#2486,12.);
#918=CIRCLE('',#2487,12.);
#919=CIRCLE('',#2490,12.);
#920=CIRCLE('',#2492,65.);
#921=CIRCLE('',#2494,65.);
#922=CIRCLE('',#2497,5.);
#923=CIRCLE('',#2499,5.);
#924=CIRCLE('',#2507,5.);
#925=CIRCLE('',#2508,5.);
#926=CIRCLE('',#2510,41.);
#927=CIRCLE('',#2511,90.);
#928=CIRCLE('',#2512,6.);
#929=CIRCLE('',#2513,90.);
#930=CIRCLE('',#2514,41.);
#931=CIRCLE('',#2515,90.);
#932=CIRCLE('',#2516,6.);
#933=CIRCLE('',#2517,90.);
#934=CIRCLE('',#2518,41.);
#935=CIRCLE('',#2519,90.);
#936=CIRCLE('',#2520,6.);
#937=CIRCLE('',#2521,90.);
#938=CIRCLE('',#2522,41.);
#939=CIRCLE('',#2523,90.);
#940=CIRCLE('',#2524,6.);
#941=CIRCLE('',#2525,90.);
#942=CIRCLE('',#2526,41.);
#943=CIRCLE('',#2527,90.);
#944=CIRCLE('',#2528,6.);
#945=CIRCLE('',#2529,90.);
#946=CIRCLE('',#2530,41.);
#947=CIRCLE('',#2531,90.);
#948=CIRCLE('',#2532,6.);
#949=CIRCLE('',#2533,90.);
#950=CIRCLE('',#2535,41.);
#951=CIRCLE('',#2537,41.);
#952=CIRCLE('',#2539,41.);
#953=CIRCLE('',#2541,41.);
#954=CIRCLE('',#2543,41.);
#955=CIRCLE('',#2545,41.);
#956=CIRCLE('',#2547,90.);
#957=CIRCLE('',#2549,90.);
#958=CIRCLE('',#2551,90.);
#959=CIRCLE('',#2553,90.);
#960=CIRCLE('',#2555,90.);
#961=CIRCLE('',#2557,90.);
#962=CIRCLE('',#2559,6.);
#963=CIRCLE('',#2560,90.);
#964=CIRCLE('',#2561,6.);
#965=CIRCLE('',#2562,90.);
#966=CIRCLE('',#2563,6.);
#967=CIRCLE('',#2564,90.);
#968=CIRCLE('',#2565,6.);
#969=CIRCLE('',#2566,90.);
#970=CIRCLE('',#2567,6.);
#971=CIRCLE('',#2568,90.);
#972=CIRCLE('',#2569,90.);
#973=CIRCLE('',#2570,6.);
#974=CIRCLE('',#2598,5.);
#975=CIRCLE('',#2602,5.);
#976=CIRCLE('',#2604,4.);
#977=CIRCLE('',#2605,4.);
#978=CIRCLE('',#2607,5.);
#979=CIRCLE('',#2609,5.);
#980=CIRCLE('',#2611,5.);
#981=CIRCLE('',#2613,8.);
#982=CIRCLE('',#2614,5.);
#983=CIRCLE('',#2616,8.);
#984=CIRCLE('',#2629,7.);
#985=CIRCLE('',#2630,5.);
#986=CIRCLE('',#2632,7.);
#987=CIRCLE('',#2633,5.);
#988=CIRCLE('',#2636,5.);
#989=CIRCLE('',#2638,4.);
#990=CIRCLE('',#2639,4.);
#991=CIRCLE('',#2641,5.);
#992=CIRCLE('',#2643,5.);
#993=CIRCLE('',#2645,5.);
#994=CIRCLE('',#2647,8.);
#995=CIRCLE('',#2649,8.);
#996=CIRCLE('',#2655,5.);
#997=CIRCLE('',#2656,5.);
#998=CIRCLE('',#2658,7.);
#999=CIRCLE('',#2659,7.);
#1000=CIRCLE('',#2664,5.);
#1001=CIRCLE('',#2665,5.);
#1002=CIRCLE('',#2667,7.);
#1003=CIRCLE('',#2668,7.);
#1004=CIRCLE('',#2673,5.);
#1005=CIRCLE('',#2674,5.);
#1006=CIRCLE('',#2676,7.);
#1007=CIRCLE('',#2677,7.);
#1008=CIRCLE('',#2682,5.);
#1009=CIRCLE('',#2683,5.);
#1010=CIRCLE('',#2685,10.);
#1011=CIRCLE('',#2686,10.);
#1012=CIRCLE('',#2693,8.);
#1013=CIRCLE('',#2694,4.);
#1014=CIRCLE('',#2696,4.);
#1015=CIRCLE('',#2698,8.);
#1016=VERTEX_POINT('',#3470);
#1017=VERTEX_POINT('',#3472);
#1018=VERTEX_POINT('',#3476);
#1019=VERTEX_POINT('',#3478);
#1020=VERTEX_POINT('',#3482);
#1021=VERTEX_POINT('',#3484);
#1022=VERTEX_POINT('',#3488);
#1023=VERTEX_POINT('',#3490);
#1024=VERTEX_POINT('',#3494);
#1025=VERTEX_POINT('',#3496);
#1026=VERTEX_POINT('',#3500);
#1027=VERTEX_POINT('',#3502);
#1028=VERTEX_POINT('',#3506);
#1029=VERTEX_POINT('',#3507);
#1030=VERTEX_POINT('',#3509);
#1031=VERTEX_POINT('',#3511);
#1032=VERTEX_POINT('',#3515);
#1033=VERTEX_POINT('',#3517);
#1034=VERTEX_POINT('',#3521);
#1035=VERTEX_POINT('',#3523);
#1036=VERTEX_POINT('',#3533);
#1037=VERTEX_POINT('',#3534);
#1038=VERTEX_POINT('',#3536);
#1039=VERTEX_POINT('',#3538);
#1040=VERTEX_POINT('',#3542);
#1041=VERTEX_POINT('',#3544);
#1042=VERTEX_POINT('',#3548);
#1043=VERTEX_POINT('',#3550);
#1044=VERTEX_POINT('',#3554);
#1045=VERTEX_POINT('',#3556);
#1046=VERTEX_POINT('',#3560);
#1047=VERTEX_POINT('',#3562);
#1048=VERTEX_POINT('',#3570);
#1049=VERTEX_POINT('',#3572);
#1050=VERTEX_POINT('',#3576);
#1051=VERTEX_POINT('',#3579);
#1052=VERTEX_POINT('',#3582);
#1053=VERTEX_POINT('',#3586);
#1054=VERTEX_POINT('',#3588);
#1055=VERTEX_POINT('',#3592);
#1056=VERTEX_POINT('',#3593);
#1057=VERTEX_POINT('',#3595);
#1058=VERTEX_POINT('',#3599);
#1059=VERTEX_POINT('',#3600);
#1060=VERTEX_POINT('',#3602);
#1061=VERTEX_POINT('',#3606);
#1062=VERTEX_POINT('',#3607);
#1063=VERTEX_POINT('',#3613);
#1064=VERTEX_POINT('',#3614);
#1065=VERTEX_POINT('',#3619);
#1066=VERTEX_POINT('',#3625);
#1067=VERTEX_POINT('',#3630);
#1068=VERTEX_POINT('',#3634);
#1069=VERTEX_POINT('',#3637);
#1070=VERTEX_POINT('',#3642);
#1071=VERTEX_POINT('',#3646);
#1072=VERTEX_POINT('',#3653);
#1073=VERTEX_POINT('',#3654);
#1074=VERTEX_POINT('',#3656);
#1075=VERTEX_POINT('',#3658);
#1076=VERTEX_POINT('',#3662);
#1077=VERTEX_POINT('',#3663);
#1078=VERTEX_POINT('',#3665);
#1079=VERTEX_POINT('',#3667);
#1080=VERTEX_POINT('',#3677);
#1081=VERTEX_POINT('',#3678);
#1082=VERTEX_POINT('',#3680);
#1083=VERTEX_POINT('',#3682);
#1084=VERTEX_POINT('',#3684);
#1085=VERTEX_POINT('',#3686);
#1086=VERTEX_POINT('',#3688);
#1087=VERTEX_POINT('',#3690);
#1088=VERTEX_POINT('',#3692);
#1089=VERTEX_POINT('',#3694);
#1090=VERTEX_POINT('',#3696);
#1091=VERTEX_POINT('',#3698);
#1092=VERTEX_POINT('',#3700);
#1093=VERTEX_POINT('',#3702);
#1094=VERTEX_POINT('',#3704);
#1095=VERTEX_POINT('',#3706);
#1096=VERTEX_POINT('',#3708);
#1097=VERTEX_POINT('',#3710);
#1098=VERTEX_POINT('',#3712);
#1099=VERTEX_POINT('',#3714);
#1100=VERTEX_POINT('',#3716);
#1101=VERTEX_POINT('',#3718);
#1102=VERTEX_POINT('',#3720);
#1103=VERTEX_POINT('',#3722);
#1104=VERTEX_POINT('',#3724);
#1105=VERTEX_POINT('',#3726);
#1106=VERTEX_POINT('',#3728);
#1107=VERTEX_POINT('',#3730);
#1108=VERTEX_POINT('',#3732);
#1109=VERTEX_POINT('',#3734);
#1110=VERTEX_POINT('',#3736);
#1111=VERTEX_POINT('',#3738);
#1112=VERTEX_POINT('',#3740);
#1113=VERTEX_POINT('',#3742);
#1114=VERTEX_POINT('',#3744);
#1115=VERTEX_POINT('',#3746);
#1116=VERTEX_POINT('',#3750);
#1117=VERTEX_POINT('',#3752);
#1118=VERTEX_POINT('',#3756);
#1119=VERTEX_POINT('',#3758);
#1120=VERTEX_POINT('',#3762);
#1121=VERTEX_POINT('',#3764);
#1122=VERTEX_POINT('',#3768);
#1123=VERTEX_POINT('',#3770);
#1124=VERTEX_POINT('',#3774);
#1125=VERTEX_POINT('',#3776);
#1126=VERTEX_POINT('',#3780);
#1127=VERTEX_POINT('',#3782);
#1128=VERTEX_POINT('',#3786);
#1129=VERTEX_POINT('',#3790);
#1130=VERTEX_POINT('',#3794);
#1131=VERTEX_POINT('',#3798);
#1132=VERTEX_POINT('',#3802);
#1133=VERTEX_POINT('',#3806);
#1134=VERTEX_POINT('',#3810);
#1135=VERTEX_POINT('',#3812);
#1136=VERTEX_POINT('',#3814);
#1137=VERTEX_POINT('',#3817);
#1138=VERTEX_POINT('',#3819);
#1139=VERTEX_POINT('',#3821);
#1140=VERTEX_POINT('',#3824);
#1141=VERTEX_POINT('',#3826);
#1142=VERTEX_POINT('',#3828);
#1143=VERTEX_POINT('',#3831);
#1144=VERTEX_POINT('',#3833);
#1145=VERTEX_POINT('',#3835);
#1146=VERTEX_POINT('',#3838);
#1147=VERTEX_POINT('',#3840);
#1148=VERTEX_POINT('',#3842);
#1149=VERTEX_POINT('',#3845);
#1150=VERTEX_POINT('',#3847);
#1151=VERTEX_POINT('',#3849);
#1152=VERTEX_POINT('',#3896);
#1153=VERTEX_POINT('',#3897);
#1154=VERTEX_POINT('',#3899);
#1155=VERTEX_POINT('',#3901);
#1156=VERTEX_POINT('',#3905);
#1157=VERTEX_POINT('',#3907);
#1158=VERTEX_POINT('',#3911);
#1159=VERTEX_POINT('',#3913);
#1160=VERTEX_POINT('',#3921);
#1161=VERTEX_POINT('',#3923);
#1162=VERTEX_POINT('',#3927);
#1163=VERTEX_POINT('',#3930);
#1164=VERTEX_POINT('',#3933);
#1165=VERTEX_POINT('',#3937);
#1166=VERTEX_POINT('',#3939);
#1167=VERTEX_POINT('',#3942);
#1168=VERTEX_POINT('',#3951);
#1169=VERTEX_POINT('',#3952);
#1170=VERTEX_POINT('',#3954);
#1171=VERTEX_POINT('',#3956);
#1172=VERTEX_POINT('',#3960);
#1173=VERTEX_POINT('',#3962);
#1174=VERTEX_POINT('',#3966);
#1175=VERTEX_POINT('',#3968);
#1176=VERTEX_POINT('',#3978);
#1177=VERTEX_POINT('',#3980);
#1178=VERTEX_POINT('',#3983);
#1179=VERTEX_POINT('',#3985);
#1180=VERTEX_POINT('',#3990);
#1181=VERTEX_POINT('',#3994);
#1182=VERTEX_POINT('',#3996);
#1183=VERTEX_POINT('',#4000);
#1184=VERTEX_POINT('',#4003);
#1185=VERTEX_POINT('',#4006);
#1186=VERTEX_POINT('',#4010);
#1187=VERTEX_POINT('',#4013);
#1188=VERTEX_POINT('',#4022);
#1189=VERTEX_POINT('',#4024);
#1190=VERTEX_POINT('',#4028);
#1191=VERTEX_POINT('',#4030);
#1192=VERTEX_POINT('',#4037);
#1193=VERTEX_POINT('',#4039);
#1194=VERTEX_POINT('',#4043);
#1195=VERTEX_POINT('',#4045);
#1196=VERTEX_POINT('',#4052);
#1197=VERTEX_POINT('',#4054);
#1198=VERTEX_POINT('',#4058);
#1199=VERTEX_POINT('',#4060);
#1200=VERTEX_POINT('',#4067);
#1201=VERTEX_POINT('',#4069);
#1202=VERTEX_POINT('',#4073);
#1203=VERTEX_POINT('',#4075);
#1204=VERTEX_POINT('',#4082);
#1205=VERTEX_POINT('',#4083);
#1206=VERTEX_POINT('',#4085);
#1207=VERTEX_POINT('',#4087);
#1208=VERTEX_POINT('',#4091);
#1209=VERTEX_POINT('',#4092);
#1210=VERTEX_POINT('',#4094);
#1211=VERTEX_POINT('',#4096);
#1212=EDGE_CURVE('',#1016,#1016,#892,.T.);
#1213=EDGE_CURVE('',#1016,#1017,#548,.T.);
#1214=EDGE_CURVE('',#1017,#1017,#893,.T.);
#1215=EDGE_CURVE('',#1018,#1018,#894,.T.);
#1216=EDGE_CURVE('',#1018,#1019,#549,.T.);
#1217=EDGE_CURVE('',#1019,#1019,#895,.T.);
#1218=EDGE_CURVE('',#1020,#1020,#896,.T.);
#1219=EDGE_CURVE('',#1020,#1021,#550,.T.);
#1220=EDGE_CURVE('',#1021,#1021,#897,.T.);
#1221=EDGE_CURVE('',#1022,#1022,#898,.T.);
#1222=EDGE_CURVE('',#1022,#1023,#551,.T.);
#1223=EDGE_CURVE('',#1023,#1023,#899,.T.);
#1224=EDGE_CURVE('',#1024,#1024,#900,.T.);
#1225=EDGE_CURVE('',#1024,#1025,#552,.T.);
#1226=EDGE_CURVE('',#1025,#1025,#901,.T.);
#1227=EDGE_CURVE('',#1026,#1026,#902,.T.);
#1228=EDGE_CURVE('',#1026,#1027,#553,.T.);
#1229=EDGE_CURVE('',#1027,#1027,#903,.T.);
#1230=EDGE_CURVE('',#1028,#1029,#554,.F.);
#1231=EDGE_CURVE('',#1029,#1030,#555,.F.);
#1232=EDGE_CURVE('',#1031,#1030,#556,.F.);
#1233=EDGE_CURVE('',#1028,#1031,#557,.F.);
#1234=EDGE_CURVE('',#1032,#1028,#558,.F.);
#1235=EDGE_CURVE('',#1033,#1031,#559,.F.);
#1236=EDGE_CURVE('',#1032,#1033,#560,.F.);
#1237=EDGE_CURVE('',#1034,#1032,#561,.F.);
#1238=EDGE_CURVE('',#1035,#1033,#562,.F.);
#1239=EDGE_CURVE('',#1034,#1035,#563,.T.);
#1240=EDGE_CURVE('',#1029,#1034,#564,.F.);
#1241=EDGE_CURVE('',#1030,#1035,#565,.F.);
#1242=EDGE_CURVE('',#1036,#1037,#566,.T.);
#1243=EDGE_CURVE('',#1036,#1038,#567,.T.);
#1244=EDGE_CURVE('',#1039,#1038,#568,.T.);
#1245=EDGE_CURVE('',#1037,#1039,#569,.T.);
#1246=EDGE_CURVE('',#1037,#1040,#570,.T.);
#1247=EDGE_CURVE('',#1041,#1039,#571,.T.);
#1248=EDGE_CURVE('',#1040,#1041,#572,.T.);
#1249=EDGE_CURVE('',#1040,#1042,#573,.T.);
#1250=EDGE_CURVE('',#1043,#1041,#574,.T.);
#1251=EDGE_CURVE('',#1042,#1043,#575,.T.);
#1252=EDGE_CURVE('',#1042,#1044,#576,.T.);
#1253=EDGE_CURVE('',#1045,#1043,#577,.T.);
#1254=EDGE_CURVE('',#1044,#1045,#578,.T.);
#1255=EDGE_CURVE('',#1044,#1046,#579,.T.);
#1256=EDGE_CURVE('',#1047,#1045,#580,.T.);
#1257=EDGE_CURVE('',#1046,#1047,#581,.T.);
#1258=EDGE_CURVE('',#1046,#1036,#582,.T.);
#1259=EDGE_CURVE('',#1038,#1047,#583,.T.);
#1260=EDGE_CURVE('',#1048,#1048,#904,.T.);
#1261=EDGE_CURVE('',#1048,#1049,#584,.T.);
#1262=EDGE_CURVE('',#1049,#1049,#905,.T.);
#1263=EDGE_CURVE('',#1050,#1050,#906,.T.);
#1264=EDGE_CURVE('',#1051,#1051,#907,.T.);
#1265=EDGE_CURVE('',#1052,#1052,#908,.T.);
#1266=EDGE_CURVE('',#1052,#1051,#585,.T.);
#1267=EDGE_CURVE('',#1053,#1053,#909,.T.);
#1268=EDGE_CURVE('',#1053,#1054,#586,.T.);
#1269=EDGE_CURVE('',#1054,#1054,#910,.T.);
#1270=EDGE_CURVE('',#1055,#1056,#911,.T.);
#1271=EDGE_CURVE('',#1057,#1055,#587,.T.);
#1272=EDGE_CURVE('',#1056,#1057,#588,.T.);
#1273=EDGE_CURVE('',#1058,#1059,#912,.T.);
#1274=EDGE_CURVE('',#1060,#1059,#589,.T.);
#1275=EDGE_CURVE('',#1058,#1060,#590,.T.);
#1276=EDGE_CURVE('',#1061,#1062,#591,.T.);
#1277=EDGE_CURVE('',#1056,#1061,#592,.T.);
#1278=EDGE_CURVE('',#1057,#1060,#593,.T.);
#1279=EDGE_CURVE('',#1062,#1059,#594,.T.);
#1280=EDGE_CURVE('',#1063,#1064,#595,.T.);
#1281=EDGE_CURVE('',#1058,#1063,#596,.T.);
#1282=EDGE_CURVE('',#1064,#1055,#597,.T.);
#1283=EDGE_CURVE('',#1065,#1055,#913,.T.);
#1284=EDGE_CURVE('',#1056,#1065,#914,.T.);
#1285=EDGE_CURVE('',#1061,#1064,#915,.T.);
#1286=EDGE_CURVE('',#1062,#1063,#916,.T.);
#1287=EDGE_CURVE('',#1059,#1066,#917,.T.);
#1288=EDGE_CURVE('',#1066,#1058,#918,.T.);
#1289=EDGE_CURVE('',#1066,#1067,#598,.T.);
#1290=EDGE_CURVE('',#1067,#1067,#919,.T.);
#1291=EDGE_CURVE('',#1068,#1068,#920,.F.);
#1292=EDGE_CURVE('',#1069,#1069,#921,.F.);
#1293=EDGE_CURVE('',#1068,#1069,#599,.T.);
#1294=EDGE_CURVE('',#1050,#1070,#600,.T.);
#1295=EDGE_CURVE('',#1070,#1070,#922,.T.);
#1296=EDGE_CURVE('',#1071,#1071,#923,.T.);
#1297=EDGE_CURVE('',#1071,#1065,#601,.T.);
#1298=EDGE_CURVE('',#1072,#1073,#602,.T.);
#1299=EDGE_CURVE('',#1074,#1072,#603,.T.);
#1300=EDGE_CURVE('',#1075,#1074,#604,.T.);
#1301=EDGE_CURVE('',#1073,#1075,#605,.T.);
#1302=EDGE_CURVE('',#1076,#1077,#606,.T.);
#1303=EDGE_CURVE('',#1078,#1076,#607,.T.);
#1304=EDGE_CURVE('',#1078,#1079,#608,.T.);
#1305=EDGE_CURVE('',#1077,#1079,#609,.T.);
#1306=EDGE_CURVE('',#1075,#1078,#610,.T.);
#1307=EDGE_CURVE('',#1079,#1074,#611,.T.);
#1308=EDGE_CURVE('',#1076,#1073,#924,.T.);
#1309=EDGE_CURVE('',#1077,#1072,#925,.T.);
#1310=EDGE_CURVE('',#1080,#1081,#926,.T.);
#1311=EDGE_CURVE('',#1081,#1082,#927,.T.);
#1312=EDGE_CURVE('',#1082,#1083,#612,.T.);
#1313=EDGE_CURVE('',#1083,#1084,#928,.T.);
#1314=EDGE_CURVE('',#1084,#1085,#613,.T.);
#1315=EDGE_CURVE('',#1085,#1086,#929,.T.);
#1316=EDGE_CURVE('',#1086,#1087,#930,.T.);
#1317=EDGE_CURVE('',#1087,#1088,#931,.T.);
#1318=EDGE_CURVE('',#1088,#1089,#614,.T.);
#1319=EDGE_CURVE('',#1089,#1090,#932,.T.);
#1320=EDGE_CURVE('',#1090,#1091,#615,.T.);
#1321=EDGE_CURVE('',#1091,#1092,#933,.T.);
#1322=EDGE_CURVE('',#1092,#1093,#934,.T.);
#1323=EDGE_CURVE('',#1093,#1094,#935,.T.);
#1324=EDGE_CURVE('',#1094,#1095,#616,.T.);
#1325=EDGE_CURVE('',#1095,#1096,#936,.T.);
#1326=EDGE_CURVE('',#1096,#1097,#617,.T.);
#1327=EDGE_CURVE('',#1097,#1098,#937,.T.);
#1328=EDGE_CURVE('',#1098,#1099,#938,.T.);
#1329=EDGE_CURVE('',#1099,#1100,#939,.T.);
#1330=EDGE_CURVE('',#1100,#1101,#618,.T.);
#1331=EDGE_CURVE('',#1101,#1102,#940,.T.);
#1332=EDGE_CURVE('',#1102,#1103,#619,.T.);
#1333=EDGE_CURVE('',#1103,#1104,#941,.T.);
#1334=EDGE_CURVE('',#1104,#1105,#942,.T.);
#1335=EDGE_CURVE('',#1105,#1106,#943,.T.);
#1336=EDGE_CURVE('',#1106,#1107,#620,.T.);
#1337=EDGE_CURVE('',#1107,#1108,#944,.T.);
#1338=EDGE_CURVE('',#1108,#1109,#621,.T.);
#1339=EDGE_CURVE('',#1109,#1110,#945,.T.);
#1340=EDGE_CURVE('',#1110,#1111,#946,.T.);
#1341=EDGE_CURVE('',#1111,#1112,#947,.T.);
#1342=EDGE_CURVE('',#1112,#1113,#622,.T.);
#1343=EDGE_CURVE('',#1113,#1114,#948,.T.);
#1344=EDGE_CURVE('',#1114,#1115,#623,.T.);
#1345=EDGE_CURVE('',#1115,#1080,#949,.T.);
#1346=EDGE_CURVE('',#1081,#1116,#624,.T.);
#1347=EDGE_CURVE('',#1117,#1080,#625,.T.);
#1348=EDGE_CURVE('',#1116,#1117,#950,.T.);
#1349=EDGE_CURVE('',#1105,#1118,#626,.T.);
#1350=EDGE_CURVE('',#1119,#1104,#627,.T.);
#1351=EDGE_CURVE('',#1118,#1119,#951,.T.);
#1352=EDGE_CURVE('',#1093,#1120,#628,.T.);
#1353=EDGE_CURVE('',#1121,#1092,#629,.T.);
#1354=EDGE_CURVE('',#1120,#1121,#952,.T.);
#1355=EDGE_CURVE('',#1099,#1122,#630,.T.);
#1356=EDGE_CURVE('',#1123,#1098,#631,.T.);
#1357=EDGE_CURVE('',#1122,#1123,#953,.T.);
#1358=EDGE_CURVE('',#1111,#1124,#632,.T.);
#1359=EDGE_CURVE('',#1125,#1110,#633,.T.);
#1360=EDGE_CURVE('',#1124,#1125,#954,.T.);
#1361=EDGE_CURVE('',#1126,#1086,#634,.T.);
#1362=EDGE_CURVE('',#1127,#1126,#955,.T.);
#1363=EDGE_CURVE('',#1087,#1127,#635,.T.);
#1364=EDGE_CURVE('',#1115,#1128,#636,.T.);
#1365=EDGE_CURVE('',#1128,#1117,#956,.T.);
#1366=EDGE_CURVE('',#1116,#1129,#957,.T.);
#1367=EDGE_CURVE('',#1129,#1082,#637,.T.);
#1368=EDGE_CURVE('',#1103,#1130,#638,.T.);
#1369=EDGE_CURVE('',#1130,#1119,#958,.T.);
#1370=EDGE_CURVE('',#1091,#1131,#639,.T.);
#1371=EDGE_CURVE('',#1131,#1121,#959,.T.);
#1372=EDGE_CURVE('',#1097,#1132,#640,.T.);
#1373=EDGE_CURVE('',#1132,#1123,#960,.T.);
#1374=EDGE_CURVE('',#1109,#1133,#641,.T.);
#1375=EDGE_CURVE('',#1133,#1125,#961,.T.);
#1376=EDGE_CURVE('',#1128,#1134,#642,.T.);
#1377=EDGE_CURVE('',#1134,#1135,#962,.T.);
#1378=EDGE_CURVE('',#1135,#1136,#643,.T.);
#1379=EDGE_CURVE('',#1124,#1136,#963,.T.);
#1380=EDGE_CURVE('',#1133,#1137,#644,.T.);
#1381=EDGE_CURVE('',#1137,#1138,#964,.T.);
#1382=EDGE_CURVE('',#1138,#1139,#645,.T.);
#1383=EDGE_CURVE('',#1118,#1139,#965,.T.);
#1384=EDGE_CURVE('',#1130,#1140,#646,.T.);
#1385=EDGE_CURVE('',#1140,#1141,#966,.T.);
#1386=EDGE_CURVE('',#1141,#1142,#647,.T.);
#1387=EDGE_CURVE('',#1122,#1142,#967,.T.);
#1388=EDGE_CURVE('',#1132,#1143,#648,.T.);
#1389=EDGE_CURVE('',#1143,#1144,#968,.T.);
#1390=EDGE_CURVE('',#1144,#1145,#649,.T.);
#1391=EDGE_CURVE('',#1120,#1145,#969,.T.);
#1392=EDGE_CURVE('',#1131,#1146,#650,.T.);
#1393=EDGE_CURVE('',#1146,#1147,#970,.T.);
#1394=EDGE_CURVE('',#1147,#1148,#651,.T.);
#1395=EDGE_CURVE('',#1127,#1148,#971,.T.);
#1396=EDGE_CURVE('',#1149,#1126,#972,.T.);
#1397=EDGE_CURVE('',#1149,#1150,#652,.T.);
#1398=EDGE_CURVE('',#1150,#1151,#973,.T.);
#1399=EDGE_CURVE('',#1151,#1129,#653,.T.);
#1400=EDGE_CURVE('',#1148,#1088,#654,.T.);
#1401=EDGE_CURVE('',#1085,#1149,#655,.T.);
#1402=EDGE_CURVE('',#1083,#1151,#656,.T.);
#1403=EDGE_CURVE('',#1084,#1150,#657,.T.);
#1404=EDGE_CURVE('',#1136,#1112,#658,.T.);
#1405=EDGE_CURVE('',#1113,#1135,#659,.T.);
#1406=EDGE_CURVE('',#1114,#1134,#660,.T.);
#1407=EDGE_CURVE('',#1139,#1106,#661,.T.);
#1408=EDGE_CURVE('',#1107,#1138,#662,.T.);
#1409=EDGE_CURVE('',#1108,#1137,#663,.T.);
#1410=EDGE_CURVE('',#1142,#1100,#664,.T.);
#1411=EDGE_CURVE('',#1101,#1141,#665,.T.);
#1412=EDGE_CURVE('',#1102,#1140,#666,.T.);
#1413=EDGE_CURVE('',#1145,#1094,#667,.T.);
#1414=EDGE_CURVE('',#1095,#1144,#668,.T.);
#1415=EDGE_CURVE('',#1096,#1143,#669,.T.);
#1416=EDGE_CURVE('',#1089,#1147,#670,.T.);
#1417=EDGE_CURVE('',#1090,#1146,#671,.T.);
#1418=EDGE_CURVE('',#1152,#1153,#672,.T.);
#1419=EDGE_CURVE('',#1152,#1154,#673,.T.);
#1420=EDGE_CURVE('',#1155,#1154,#674,.T.);
#1421=EDGE_CURVE('',#1155,#1153,#675,.T.);
#1422=EDGE_CURVE('',#1153,#1156,#974,.T.);
#1423=EDGE_CURVE('',#1157,#1155,#676,.T.);
#1424=EDGE_CURVE('',#1156,#1157,#677,.T.);
#1425=EDGE_CURVE('',#1156,#1158,#678,.T.);
#1426=EDGE_CURVE('',#1157,#1159,#679,.T.);
#1427=EDGE_CURVE('',#1159,#1158,#680,.T.);
#1428=EDGE_CURVE('',#1154,#1159,#681,.T.);
#1429=EDGE_CURVE('',#1158,#1152,#975,.T.);
#1430=EDGE_CURVE('',#1160,#1160,#976,.T.);
#1431=EDGE_CURVE('',#1160,#1161,#682,.T.);
#1432=EDGE_CURVE('',#1161,#1161,#977,.T.);
#1433=EDGE_CURVE('',#1162,#1162,#978,.T.);
#1434=EDGE_CURVE('',#1163,#1163,#979,.T.);
#1435=EDGE_CURVE('',#1164,#1164,#980,.T.);
#1436=EDGE_CURVE('',#1164,#1163,#683,.T.);
#1437=EDGE_CURVE('',#1165,#1165,#981,.T.);
#1438=EDGE_CURVE('',#1166,#1166,#982,.T.);
#1439=EDGE_CURVE('',#1165,#1167,#684,.T.);
#1440=EDGE_CURVE('',#1167,#1167,#983,.T.);
#1441=EDGE_CURVE('',#1162,#1166,#685,.T.);
#1442=EDGE_CURVE('',#1168,#1169,#686,.T.);
#1443=EDGE_CURVE('',#1169,#1170,#687,.T.);
#1444=EDGE_CURVE('',#1171,#1170,#688,.T.);
#1445=EDGE_CURVE('',#1168,#1171,#689,.T.);
#1446=EDGE_CURVE('',#1172,#1168,#690,.T.);
#1447=EDGE_CURVE('',#1173,#1171,#691,.T.);
#1448=EDGE_CURVE('',#1172,#1173,#692,.T.);
#1449=EDGE_CURVE('',#1174,#1172,#693,.T.);
#1450=EDGE_CURVE('',#1175,#1173,#694,.T.);
#1451=EDGE_CURVE('',#1174,#1175,#695,.T.);
#1452=EDGE_CURVE('',#1169,#1174,#696,.T.);
#1453=EDGE_CURVE('',#1170,#1175,#697,.T.);
#1454=EDGE_CURVE('',#1176,#1176,#984,.T.);
#1455=EDGE_CURVE('',#1177,#1177,#985,.T.);
#1456=EDGE_CURVE('',#1178,#1178,#986,.T.);
#1457=EDGE_CURVE('',#1179,#1179,#987,.T.);
#1458=EDGE_CURVE('',#1176,#1178,#698,.T.);
#1459=EDGE_CURVE('',#1179,#1180,#699,.T.);
#1460=EDGE_CURVE('',#1180,#1180,#988,.T.);
#1461=EDGE_CURVE('',#1181,#1181,#989,.T.);
#1462=EDGE_CURVE('',#1181,#1182,#700,.T.);
#1463=EDGE_CURVE('',#1182,#1182,#990,.T.);
#1464=EDGE_CURVE('',#1183,#1183,#991,.T.);
#1465=EDGE_CURVE('',#1184,#1184,#992,.T.);
#1466=EDGE_CURVE('',#1185,#1185,#993,.T.);
#1467=EDGE_CURVE('',#1185,#1184,#701,.T.);
#1468=EDGE_CURVE('',#1186,#1186,#994,.T.);
#1469=EDGE_CURVE('',#1186,#1187,#702,.T.);
#1470=EDGE_CURVE('',#1187,#1187,#995,.T.);
#1471=EDGE_CURVE('',#1183,#1177,#703,.T.);
#1472=EDGE_CURVE('',#1188,#1188,#996,.T.);
#1473=EDGE_CURVE('',#1188,#1189,#704,.T.);
#1474=EDGE_CURVE('',#1189,#1189,#997,.T.);
#1475=EDGE_CURVE('',#1190,#1190,#998,.T.);
#1476=EDGE_CURVE('',#1190,#1191,#705,.T.);
#1477=EDGE_CURVE('',#1191,#1191,#999,.T.);
#1478=EDGE_CURVE('',#1192,#1192,#1000,.T.);
#1479=EDGE_CURVE('',#1192,#1193,#706,.T.);
#1480=EDGE_CURVE('',#1193,#1193,#1001,.T.);
#1481=EDGE_CURVE('',#1194,#1194,#1002,.T.);
#1482=EDGE_CURVE('',#1194,#1195,#707,.T.);
#1483=EDGE_CURVE('',#1195,#1195,#1003,.T.);
#1484=EDGE_CURVE('',#1196,#1196,#1004,.T.);
#1485=EDGE_CURVE('',#1196,#1197,#708,.T.);
#1486=EDGE_CURVE('',#1197,#1197,#1005,.T.);
#1487=EDGE_CURVE('',#1198,#1198,#1006,.T.);
#1488=EDGE_CURVE('',#1198,#1199,#709,.T.);
#1489=EDGE_CURVE('',#1199,#1199,#1007,.T.);
#1490=EDGE_CURVE('',#1200,#1200,#1008,.T.);
#1491=EDGE_CURVE('',#1200,#1201,#710,.T.);
#1492=EDGE_CURVE('',#1201,#1201,#1009,.T.);
#1493=EDGE_CURVE('',#1202,#1202,#1010,.T.);
#1494=EDGE_CURVE('',#1202,#1203,#711,.T.);
#1495=EDGE_CURVE('',#1203,#1203,#1011,.T.);
#1496=EDGE_CURVE('',#1204,#1205,#712,.T.);
#1497=EDGE_CURVE('',#1206,#1204,#713,.T.);
#1498=EDGE_CURVE('',#1207,#1206,#714,.T.);
#1499=EDGE_CURVE('',#1205,#1207,#715,.T.);
#1500=EDGE_CURVE('',#1208,#1209,#716,.T.);
#1501=EDGE_CURVE('',#1210,#1208,#717,.T.);
#1502=EDGE_CURVE('',#1211,#1210,#718,.T.);
#1503=EDGE_CURVE('',#1209,#1211,#719,.T.);
#1504=EDGE_CURVE('',#1206,#1211,#1012,.T.);
#1505=EDGE_CURVE('',#1209,#1204,#1013,.T.);
#1506=EDGE_CURVE('',#1208,#1205,#1014,.T.);
#1507=EDGE_CURVE('',#1207,#1210,#1015,.T.);
#1508=ORIENTED_EDGE('',*,*,#1212,.F.);
#1509=ORIENTED_EDGE('',*,*,#1213,.T.);
#1510=ORIENTED_EDGE('',*,*,#1214,.F.);
#1511=ORIENTED_EDGE('',*,*,#1213,.F.);
#1512=ORIENTED_EDGE('',*,*,#1215,.F.);
#1513=ORIENTED_EDGE('',*,*,#1216,.T.);
#1514=ORIENTED_EDGE('',*,*,#1217,.F.);
#1515=ORIENTED_EDGE('',*,*,#1216,.F.);
#1516=ORIENTED_EDGE('',*,*,#1218,.F.);
#1517=ORIENTED_EDGE('',*,*,#1219,.T.);
#1518=ORIENTED_EDGE('',*,*,#1220,.F.);
#1519=ORIENTED_EDGE('',*,*,#1219,.F.);
#1520=ORIENTED_EDGE('',*,*,#1221,.F.);
#1521=ORIENTED_EDGE('',*,*,#1222,.T.);
#1522=ORIENTED_EDGE('',*,*,#1223,.F.);
#1523=ORIENTED_EDGE('',*,*,#1222,.F.);
#1524=ORIENTED_EDGE('',*,*,#1224,.F.);
#1525=ORIENTED_EDGE('',*,*,#1225,.T.);
#1526=ORIENTED_EDGE('',*,*,#1226,.F.);
#1527=ORIENTED_EDGE('',*,*,#1225,.F.);
#1528=ORIENTED_EDGE('',*,*,#1227,.F.);
#1529=ORIENTED_EDGE('',*,*,#1228,.T.);
#1530=ORIENTED_EDGE('',*,*,#1229,.F.);
#1531=ORIENTED_EDGE('',*,*,#1228,.F.);
#1532=ORIENTED_EDGE('',*,*,#1230,.T.);
#1533=ORIENTED_EDGE('',*,*,#1231,.T.);
#1534=ORIENTED_EDGE('',*,*,#1232,.F.);
#1535=ORIENTED_EDGE('',*,*,#1233,.F.);
#1536=ORIENTED_EDGE('',*,*,#1234,.T.);
#1537=ORIENTED_EDGE('',*,*,#1233,.T.);
#1538=ORIENTED_EDGE('',*,*,#1235,.F.);
#1539=ORIENTED_EDGE('',*,*,#1236,.F.);
#1540=ORIENTED_EDGE('',*,*,#1237,.T.);
#1541=ORIENTED_EDGE('',*,*,#1236,.T.);
#1542=ORIENTED_EDGE('',*,*,#1238,.F.);
#1543=ORIENTED_EDGE('',*,*,#1239,.F.);
#1544=ORIENTED_EDGE('',*,*,#1240,.T.);
#1545=ORIENTED_EDGE('',*,*,#1239,.T.);
#1546=ORIENTED_EDGE('',*,*,#1241,.F.);
#1547=ORIENTED_EDGE('',*,*,#1231,.F.);
#1548=ORIENTED_EDGE('',*,*,#1241,.T.);
#1549=ORIENTED_EDGE('',*,*,#1238,.T.);
#1550=ORIENTED_EDGE('',*,*,#1235,.T.);
#1551=ORIENTED_EDGE('',*,*,#1232,.T.);
#1552=ORIENTED_EDGE('',*,*,#1227,.T.);
#1553=ORIENTED_EDGE('',*,*,#1224,.T.);
#1554=ORIENTED_EDGE('',*,*,#1221,.T.);
#1555=ORIENTED_EDGE('',*,*,#1218,.T.);
#1556=ORIENTED_EDGE('',*,*,#1215,.T.);
#1557=ORIENTED_EDGE('',*,*,#1212,.T.);
#1558=ORIENTED_EDGE('',*,*,#1240,.F.);
#1559=ORIENTED_EDGE('',*,*,#1230,.F.);
#1560=ORIENTED_EDGE('',*,*,#1234,.F.);
#1561=ORIENTED_EDGE('',*,*,#1237,.F.);
#1562=ORIENTED_EDGE('',*,*,#1229,.T.);
#1563=ORIENTED_EDGE('',*,*,#1226,.T.);
#1564=ORIENTED_EDGE('',*,*,#1223,.T.);
#1565=ORIENTED_EDGE('',*,*,#1220,.T.);
#1566=ORIENTED_EDGE('',*,*,#1217,.T.);
#1567=ORIENTED_EDGE('',*,*,#1214,.T.);
#1568=ORIENTED_EDGE('',*,*,#1242,.F.);
#1569=ORIENTED_EDGE('',*,*,#1243,.T.);
#1570=ORIENTED_EDGE('',*,*,#1244,.F.);
#1571=ORIENTED_EDGE('',*,*,#1245,.F.);
#1572=ORIENTED_EDGE('',*,*,#1246,.F.);
#1573=ORIENTED_EDGE('',*,*,#1245,.T.);
#1574=ORIENTED_EDGE('',*,*,#1247,.F.);
#1575=ORIENTED_EDGE('',*,*,#1248,.F.);
#1576=ORIENTED_EDGE('',*,*,#1249,.F.);
#1577=ORIENTED_EDGE('',*,*,#1248,.T.);
#1578=ORIENTED_EDGE('',*,*,#1250,.F.);
#1579=ORIENTED_EDGE('',*,*,#1251,.F.);
#1580=ORIENTED_EDGE('',*,*,#1252,.F.);
#1581=ORIENTED_EDGE('',*,*,#1251,.T.);
#1582=ORIENTED_EDGE('',*,*,#1253,.F.);
#1583=ORIENTED_EDGE('',*,*,#1254,.F.);
#1584=ORIENTED_EDGE('',*,*,#1255,.F.);
#1585=ORIENTED_EDGE('',*,*,#1254,.T.);
#1586=ORIENTED_EDGE('',*,*,#1256,.F.);
#1587=ORIENTED_EDGE('',*,*,#1257,.F.);
#1588=ORIENTED_EDGE('',*,*,#1258,.F.);
#1589=ORIENTED_EDGE('',*,*,#1257,.T.);
#1590=ORIENTED_EDGE('',*,*,#1259,.F.);
#1591=ORIENTED_EDGE('',*,*,#1243,.F.);
#1592=ORIENTED_EDGE('',*,*,#1259,.T.);
#1593=ORIENTED_EDGE('',*,*,#1256,.T.);
#1594=ORIENTED_EDGE('',*,*,#1253,.T.);
#1595=ORIENTED_EDGE('',*,*,#1250,.T.);
#1596=ORIENTED_EDGE('',*,*,#1247,.T.);
#1597=ORIENTED_EDGE('',*,*,#1244,.T.);
#1598=ORIENTED_EDGE('',*,*,#1260,.T.);
#1599=ORIENTED_EDGE('',*,*,#1261,.T.);
#1600=ORIENTED_EDGE('',*,*,#1262,.F.);
#1601=ORIENTED_EDGE('',*,*,#1261,.F.);
#1602=ORIENTED_EDGE('',*,*,#1263,.F.);
#1603=ORIENTED_EDGE('',*,*,#1260,.F.);
#1604=ORIENTED_EDGE('',*,*,#1264,.F.);
#1605=ORIENTED_EDGE('',*,*,#1262,.T.);
#1606=ORIENTED_EDGE('',*,*,#1265,.T.);
#1607=ORIENTED_EDGE('',*,*,#1266,.T.);
#1608=ORIENTED_EDGE('',*,*,#1264,.T.);
#1609=ORIENTED_EDGE('',*,*,#1266,.F.);
#1610=ORIENTED_EDGE('',*,*,#1267,.F.);
#1611=ORIENTED_EDGE('',*,*,#1268,.T.);
#1612=ORIENTED_EDGE('',*,*,#1269,.F.);
#1613=ORIENTED_EDGE('',*,*,#1268,.F.);
#1614=ORIENTED_EDGE('',*,*,#1270,.F.);
#1615=ORIENTED_EDGE('',*,*,#1271,.F.);
#1616=ORIENTED_EDGE('',*,*,#1272,.F.);
#1617=ORIENTED_EDGE('',*,*,#1273,.T.);
#1618=ORIENTED_EDGE('',*,*,#1274,.F.);
#1619=ORIENTED_EDGE('',*,*,#1275,.F.);
#1620=ORIENTED_EDGE('',*,*,#1276,.F.);
#1621=ORIENTED_EDGE('',*,*,#1277,.F.);
#1622=ORIENTED_EDGE('',*,*,#1272,.T.);
#1623=ORIENTED_EDGE('',*,*,#1278,.T.);
#1624=ORIENTED_EDGE('',*,*,#1274,.T.);
#1625=ORIENTED_EDGE('',*,*,#1279,.F.);
#1626=ORIENTED_EDGE('',*,*,#1280,.F.);
#1627=ORIENTED_EDGE('',*,*,#1281,.F.);
#1628=ORIENTED_EDGE('',*,*,#1275,.T.);
#1629=ORIENTED_EDGE('',*,*,#1278,.F.);
#1630=ORIENTED_EDGE('',*,*,#1271,.T.);
#1631=ORIENTED_EDGE('',*,*,#1282,.F.);
#1632=ORIENTED_EDGE('',*,*,#1282,.T.);
#1633=ORIENTED_EDGE('',*,*,#1283,.F.);
#1634=ORIENTED_EDGE('',*,*,#1284,.F.);
#1635=ORIENTED_EDGE('',*,*,#1277,.T.);
#1636=ORIENTED_EDGE('',*,*,#1285,.T.);
#1637=ORIENTED_EDGE('',*,*,#1281,.T.);
#1638=ORIENTED_EDGE('',*,*,#1286,.F.);
#1639=ORIENTED_EDGE('',*,*,#1279,.T.);
#1640=ORIENTED_EDGE('',*,*,#1287,.T.);
#1641=ORIENTED_EDGE('',*,*,#1288,.T.);
#1642=ORIENTED_EDGE('',*,*,#1280,.T.);
#1643=ORIENTED_EDGE('',*,*,#1285,.F.);
#1644=ORIENTED_EDGE('',*,*,#1276,.T.);
#1645=ORIENTED_EDGE('',*,*,#1286,.T.);
#1646=ORIENTED_EDGE('',*,*,#1287,.F.);
#1647=ORIENTED_EDGE('',*,*,#1273,.F.);
#1648=ORIENTED_EDGE('',*,*,#1288,.F.);
#1649=ORIENTED_EDGE('',*,*,#1289,.T.);
#1650=ORIENTED_EDGE('',*,*,#1290,.F.);
#1651=ORIENTED_EDGE('',*,*,#1289,.F.);
#1652=ORIENTED_EDGE('',*,*,#1291,.T.);
#1653=ORIENTED_EDGE('',*,*,#1267,.T.);
#1654=ORIENTED_EDGE('',*,*,#1290,.T.);
#1655=ORIENTED_EDGE('',*,*,#1292,.F.);
#1656=ORIENTED_EDGE('',*,*,#1269,.T.);
#1657=ORIENTED_EDGE('',*,*,#1265,.F.);
#1658=ORIENTED_EDGE('',*,*,#1291,.F.);
#1659=ORIENTED_EDGE('',*,*,#1293,.T.);
#1660=ORIENTED_EDGE('',*,*,#1292,.T.);
#1661=ORIENTED_EDGE('',*,*,#1293,.F.);
#1662=ORIENTED_EDGE('',*,*,#1263,.T.);
#1663=ORIENTED_EDGE('',*,*,#1294,.T.);
#1664=ORIENTED_EDGE('',*,*,#1295,.T.);
#1665=ORIENTED_EDGE('',*,*,#1294,.F.);
#1666=ORIENTED_EDGE('',*,*,#1296,.F.);
#1667=ORIENTED_EDGE('',*,*,#1297,.T.);
#1668=ORIENTED_EDGE('',*,*,#1283,.T.);
#1669=ORIENTED_EDGE('',*,*,#1270,.T.);
#1670=ORIENTED_EDGE('',*,*,#1284,.T.);
#1671=ORIENTED_EDGE('',*,*,#1297,.F.);
#1672=ORIENTED_EDGE('',*,*,#1296,.T.);
#1673=ORIENTED_EDGE('',*,*,#1242,.T.);
#1674=ORIENTED_EDGE('',*,*,#1246,.T.);
#1675=ORIENTED_EDGE('',*,*,#1249,.T.);
#1676=ORIENTED_EDGE('',*,*,#1252,.T.);
#1677=ORIENTED_EDGE('',*,*,#1255,.T.);
#1678=ORIENTED_EDGE('',*,*,#1258,.T.);
#1679=ORIENTED_EDGE('',*,*,#1295,.F.);
#1680=ORIENTED_EDGE('',*,*,#1298,.F.);
#1681=ORIENTED_EDGE('',*,*,#1299,.F.);
#1682=ORIENTED_EDGE('',*,*,#1300,.F.);
#1683=ORIENTED_EDGE('',*,*,#1301,.F.);
#1684=ORIENTED_EDGE('',*,*,#1302,.F.);
#1685=ORIENTED_EDGE('',*,*,#1303,.F.);
#1686=ORIENTED_EDGE('',*,*,#1304,.T.);
#1687=ORIENTED_EDGE('',*,*,#1305,.F.);
#1688=ORIENTED_EDGE('',*,*,#1306,.F.);
#1689=ORIENTED_EDGE('',*,*,#1300,.T.);
#1690=ORIENTED_EDGE('',*,*,#1307,.F.);
#1691=ORIENTED_EDGE('',*,*,#1304,.F.);
#1692=ORIENTED_EDGE('',*,*,#1298,.T.);
#1693=ORIENTED_EDGE('',*,*,#1308,.F.);
#1694=ORIENTED_EDGE('',*,*,#1302,.T.);
#1695=ORIENTED_EDGE('',*,*,#1309,.T.);
#1696=ORIENTED_EDGE('',*,*,#1310,.T.);
#1697=ORIENTED_EDGE('',*,*,#1311,.T.);
#1698=ORIENTED_EDGE('',*,*,#1312,.T.);
#1699=ORIENTED_EDGE('',*,*,#1313,.T.);
#1700=ORIENTED_EDGE('',*,*,#1314,.T.);
#1701=ORIENTED_EDGE('',*,*,#1315,.T.);
#1702=ORIENTED_EDGE('',*,*,#1316,.T.);
#1703=ORIENTED_EDGE('',*,*,#1317,.T.);
#1704=ORIENTED_EDGE('',*,*,#1318,.T.);
#1705=ORIENTED_EDGE('',*,*,#1319,.T.);
#1706=ORIENTED_EDGE('',*,*,#1320,.T.);
#1707=ORIENTED_EDGE('',*,*,#1321,.T.);
#1708=ORIENTED_EDGE('',*,*,#1322,.T.);
#1709=ORIENTED_EDGE('',*,*,#1323,.T.);
#1710=ORIENTED_EDGE('',*,*,#1324,.T.);
#1711=ORIENTED_EDGE('',*,*,#1325,.T.);
#1712=ORIENTED_EDGE('',*,*,#1326,.T.);
#1713=ORIENTED_EDGE('',*,*,#1327,.T.);
#1714=ORIENTED_EDGE('',*,*,#1328,.T.);
#1715=ORIENTED_EDGE('',*,*,#1329,.T.);
#1716=ORIENTED_EDGE('',*,*,#1330,.T.);
#1717=ORIENTED_EDGE('',*,*,#1331,.T.);
#1718=ORIENTED_EDGE('',*,*,#1332,.T.);
#1719=ORIENTED_EDGE('',*,*,#1333,.T.);
#1720=ORIENTED_EDGE('',*,*,#1334,.T.);
#1721=ORIENTED_EDGE('',*,*,#1335,.T.);
#1722=ORIENTED_EDGE('',*,*,#1336,.T.);
#1723=ORIENTED_EDGE('',*,*,#1337,.T.);
#1724=ORIENTED_EDGE('',*,*,#1338,.T.);
#1725=ORIENTED_EDGE('',*,*,#1339,.T.);
#1726=ORIENTED_EDGE('',*,*,#1340,.T.);
#1727=ORIENTED_EDGE('',*,*,#1341,.T.);
#1728=ORIENTED_EDGE('',*,*,#1342,.T.);
#1729=ORIENTED_EDGE('',*,*,#1343,.T.);
#1730=ORIENTED_EDGE('',*,*,#1344,.T.);
#1731=ORIENTED_EDGE('',*,*,#1345,.T.);
#1732=ORIENTED_EDGE('',*,*,#1301,.T.);
#1733=ORIENTED_EDGE('',*,*,#1306,.T.);
#1734=ORIENTED_EDGE('',*,*,#1303,.T.);
#1735=ORIENTED_EDGE('',*,*,#1308,.T.);
#1736=ORIENTED_EDGE('',*,*,#1346,.F.);
#1737=ORIENTED_EDGE('',*,*,#1310,.F.);
#1738=ORIENTED_EDGE('',*,*,#1347,.F.);
#1739=ORIENTED_EDGE('',*,*,#1348,.F.);
#1740=ORIENTED_EDGE('',*,*,#1349,.F.);
#1741=ORIENTED_EDGE('',*,*,#1334,.F.);
#1742=ORIENTED_EDGE('',*,*,#1350,.F.);
#1743=ORIENTED_EDGE('',*,*,#1351,.F.);
#1744=ORIENTED_EDGE('',*,*,#1352,.F.);
#1745=ORIENTED_EDGE('',*,*,#1322,.F.);
#1746=ORIENTED_EDGE('',*,*,#1353,.F.);
#1747=ORIENTED_EDGE('',*,*,#1354,.F.);
#1748=ORIENTED_EDGE('',*,*,#1355,.F.);
#1749=ORIENTED_EDGE('',*,*,#1328,.F.);
#1750=ORIENTED_EDGE('',*,*,#1356,.F.);
#1751=ORIENTED_EDGE('',*,*,#1357,.F.);
#1752=ORIENTED_EDGE('',*,*,#1358,.F.);
#1753=ORIENTED_EDGE('',*,*,#1340,.F.);
#1754=ORIENTED_EDGE('',*,*,#1359,.F.);
#1755=ORIENTED_EDGE('',*,*,#1360,.F.);
#1756=ORIENTED_EDGE('',*,*,#1361,.F.);
#1757=ORIENTED_EDGE('',*,*,#1362,.F.);
#1758=ORIENTED_EDGE('',*,*,#1363,.F.);
#1759=ORIENTED_EDGE('',*,*,#1316,.F.);
#1760=ORIENTED_EDGE('',*,*,#1347,.T.);
#1761=ORIENTED_EDGE('',*,*,#1345,.F.);
#1762=ORIENTED_EDGE('',*,*,#1364,.T.);
#1763=ORIENTED_EDGE('',*,*,#1365,.T.);
#1764=ORIENTED_EDGE('',*,*,#1346,.T.);
#1765=ORIENTED_EDGE('',*,*,#1366,.T.);
#1766=ORIENTED_EDGE('',*,*,#1367,.T.);
#1767=ORIENTED_EDGE('',*,*,#1311,.F.);
#1768=ORIENTED_EDGE('',*,*,#1350,.T.);
#1769=ORIENTED_EDGE('',*,*,#1333,.F.);
#1770=ORIENTED_EDGE('',*,*,#1368,.T.);
#1771=ORIENTED_EDGE('',*,*,#1369,.T.);
#1772=ORIENTED_EDGE('',*,*,#1353,.T.);
#1773=ORIENTED_EDGE('',*,*,#1321,.F.);
#1774=ORIENTED_EDGE('',*,*,#1370,.T.);
#1775=ORIENTED_EDGE('',*,*,#1371,.T.);
#1776=ORIENTED_EDGE('',*,*,#1356,.T.);
#1777=ORIENTED_EDGE('',*,*,#1327,.F.);
#1778=ORIENTED_EDGE('',*,*,#1372,.T.);
#1779=ORIENTED_EDGE('',*,*,#1373,.T.);
#1780=ORIENTED_EDGE('',*,*,#1359,.T.);
#1781=ORIENTED_EDGE('',*,*,#1339,.F.);
#1782=ORIENTED_EDGE('',*,*,#1374,.T.);
#1783=ORIENTED_EDGE('',*,*,#1375,.T.);
#1784=ORIENTED_EDGE('',*,*,#1348,.T.);
#1785=ORIENTED_EDGE('',*,*,#1365,.F.);
#1786=ORIENTED_EDGE('',*,*,#1376,.T.);
#1787=ORIENTED_EDGE('',*,*,#1377,.T.);
#1788=ORIENTED_EDGE('',*,*,#1378,.T.);
#1789=ORIENTED_EDGE('',*,*,#1379,.F.);
#1790=ORIENTED_EDGE('',*,*,#1360,.T.);
#1791=ORIENTED_EDGE('',*,*,#1375,.F.);
#1792=ORIENTED_EDGE('',*,*,#1380,.T.);
#1793=ORIENTED_EDGE('',*,*,#1381,.T.);
#1794=ORIENTED_EDGE('',*,*,#1382,.T.);
#1795=ORIENTED_EDGE('',*,*,#1383,.F.);
#1796=ORIENTED_EDGE('',*,*,#1351,.T.);
#1797=ORIENTED_EDGE('',*,*,#1369,.F.);
#1798=ORIENTED_EDGE('',*,*,#1384,.T.);
#1799=ORIENTED_EDGE('',*,*,#1385,.T.);
#1800=ORIENTED_EDGE('',*,*,#1386,.T.);
#1801=ORIENTED_EDGE('',*,*,#1387,.F.);
#1802=ORIENTED_EDGE('',*,*,#1357,.T.);
#1803=ORIENTED_EDGE('',*,*,#1373,.F.);
#1804=ORIENTED_EDGE('',*,*,#1388,.T.);
#1805=ORIENTED_EDGE('',*,*,#1389,.T.);
#1806=ORIENTED_EDGE('',*,*,#1390,.T.);
#1807=ORIENTED_EDGE('',*,*,#1391,.F.);
#1808=ORIENTED_EDGE('',*,*,#1354,.T.);
#1809=ORIENTED_EDGE('',*,*,#1371,.F.);
#1810=ORIENTED_EDGE('',*,*,#1392,.T.);
#1811=ORIENTED_EDGE('',*,*,#1393,.T.);
#1812=ORIENTED_EDGE('',*,*,#1394,.T.);
#1813=ORIENTED_EDGE('',*,*,#1395,.F.);
#1814=ORIENTED_EDGE('',*,*,#1362,.T.);
#1815=ORIENTED_EDGE('',*,*,#1396,.F.);
#1816=ORIENTED_EDGE('',*,*,#1397,.T.);
#1817=ORIENTED_EDGE('',*,*,#1398,.T.);
#1818=ORIENTED_EDGE('',*,*,#1399,.T.);
#1819=ORIENTED_EDGE('',*,*,#1366,.F.);
#1820=ORIENTED_EDGE('',*,*,#1299,.T.);
#1821=ORIENTED_EDGE('',*,*,#1309,.F.);
#1822=ORIENTED_EDGE('',*,*,#1305,.T.);
#1823=ORIENTED_EDGE('',*,*,#1307,.T.);
#1824=ORIENTED_EDGE('',*,*,#1363,.T.);
#1825=ORIENTED_EDGE('',*,*,#1395,.T.);
#1826=ORIENTED_EDGE('',*,*,#1400,.T.);
#1827=ORIENTED_EDGE('',*,*,#1317,.F.);
#1828=ORIENTED_EDGE('',*,*,#1361,.T.);
#1829=ORIENTED_EDGE('',*,*,#1315,.F.);
#1830=ORIENTED_EDGE('',*,*,#1401,.T.);
#1831=ORIENTED_EDGE('',*,*,#1396,.T.);
#1832=ORIENTED_EDGE('',*,*,#1367,.F.);
#1833=ORIENTED_EDGE('',*,*,#1399,.F.);
#1834=ORIENTED_EDGE('',*,*,#1402,.F.);
#1835=ORIENTED_EDGE('',*,*,#1312,.F.);
#1836=ORIENTED_EDGE('',*,*,#1401,.F.);
#1837=ORIENTED_EDGE('',*,*,#1314,.F.);
#1838=ORIENTED_EDGE('',*,*,#1403,.T.);
#1839=ORIENTED_EDGE('',*,*,#1397,.F.);
#1840=ORIENTED_EDGE('',*,*,#1313,.F.);
#1841=ORIENTED_EDGE('',*,*,#1402,.T.);
#1842=ORIENTED_EDGE('',*,*,#1398,.F.);
#1843=ORIENTED_EDGE('',*,*,#1403,.F.);
#1844=ORIENTED_EDGE('',*,*,#1404,.F.);
#1845=ORIENTED_EDGE('',*,*,#1378,.F.);
#1846=ORIENTED_EDGE('',*,*,#1405,.F.);
#1847=ORIENTED_EDGE('',*,*,#1342,.F.);
#1848=ORIENTED_EDGE('',*,*,#1364,.F.);
#1849=ORIENTED_EDGE('',*,*,#1344,.F.);
#1850=ORIENTED_EDGE('',*,*,#1406,.T.);
#1851=ORIENTED_EDGE('',*,*,#1376,.F.);
#1852=ORIENTED_EDGE('',*,*,#1343,.F.);
#1853=ORIENTED_EDGE('',*,*,#1405,.T.);
#1854=ORIENTED_EDGE('',*,*,#1377,.F.);
#1855=ORIENTED_EDGE('',*,*,#1406,.F.);
#1856=ORIENTED_EDGE('',*,*,#1407,.F.);
#1857=ORIENTED_EDGE('',*,*,#1382,.F.);
#1858=ORIENTED_EDGE('',*,*,#1408,.F.);
#1859=ORIENTED_EDGE('',*,*,#1336,.F.);
#1860=ORIENTED_EDGE('',*,*,#1374,.F.);
#1861=ORIENTED_EDGE('',*,*,#1338,.F.);
#1862=ORIENTED_EDGE('',*,*,#1409,.T.);
#1863=ORIENTED_EDGE('',*,*,#1380,.F.);
#1864=ORIENTED_EDGE('',*,*,#1337,.F.);
#1865=ORIENTED_EDGE('',*,*,#1408,.T.);
#1866=ORIENTED_EDGE('',*,*,#1381,.F.);
#1867=ORIENTED_EDGE('',*,*,#1409,.F.);
#1868=ORIENTED_EDGE('',*,*,#1358,.T.);
#1869=ORIENTED_EDGE('',*,*,#1379,.T.);
#1870=ORIENTED_EDGE('',*,*,#1404,.T.);
#1871=ORIENTED_EDGE('',*,*,#1341,.F.);
#1872=ORIENTED_EDGE('',*,*,#1349,.T.);
#1873=ORIENTED_EDGE('',*,*,#1383,.T.);
#1874=ORIENTED_EDGE('',*,*,#1407,.T.);
#1875=ORIENTED_EDGE('',*,*,#1335,.F.);
#1876=ORIENTED_EDGE('',*,*,#1410,.F.);
#1877=ORIENTED_EDGE('',*,*,#1386,.F.);
#1878=ORIENTED_EDGE('',*,*,#1411,.F.);
#1879=ORIENTED_EDGE('',*,*,#1330,.F.);
#1880=ORIENTED_EDGE('',*,*,#1368,.F.);
#1881=ORIENTED_EDGE('',*,*,#1332,.F.);
#1882=ORIENTED_EDGE('',*,*,#1412,.T.);
#1883=ORIENTED_EDGE('',*,*,#1384,.F.);
#1884=ORIENTED_EDGE('',*,*,#1331,.F.);
#1885=ORIENTED_EDGE('',*,*,#1411,.T.);
#1886=ORIENTED_EDGE('',*,*,#1385,.F.);
#1887=ORIENTED_EDGE('',*,*,#1412,.F.);
#1888=ORIENTED_EDGE('',*,*,#1413,.F.);
#1889=ORIENTED_EDGE('',*,*,#1390,.F.);
#1890=ORIENTED_EDGE('',*,*,#1414,.F.);
#1891=ORIENTED_EDGE('',*,*,#1324,.F.);
#1892=ORIENTED_EDGE('',*,*,#1372,.F.);
#1893=ORIENTED_EDGE('',*,*,#1326,.F.);
#1894=ORIENTED_EDGE('',*,*,#1415,.T.);
#1895=ORIENTED_EDGE('',*,*,#1388,.F.);
#1896=ORIENTED_EDGE('',*,*,#1325,.F.);
#1897=ORIENTED_EDGE('',*,*,#1414,.T.);
#1898=ORIENTED_EDGE('',*,*,#1389,.F.);
#1899=ORIENTED_EDGE('',*,*,#1415,.F.);
#1900=ORIENTED_EDGE('',*,*,#1355,.T.);
#1901=ORIENTED_EDGE('',*,*,#1387,.T.);
#1902=ORIENTED_EDGE('',*,*,#1410,.T.);
#1903=ORIENTED_EDGE('',*,*,#1329,.F.);
#1904=ORIENTED_EDGE('',*,*,#1352,.T.);
#1905=ORIENTED_EDGE('',*,*,#1391,.T.);
#1906=ORIENTED_EDGE('',*,*,#1413,.T.);
#1907=ORIENTED_EDGE('',*,*,#1323,.F.);
#1908=ORIENTED_EDGE('',*,*,#1400,.F.);
#1909=ORIENTED_EDGE('',*,*,#1394,.F.);
#1910=ORIENTED_EDGE('',*,*,#1416,.F.);
#1911=ORIENTED_EDGE('',*,*,#1318,.F.);
#1912=ORIENTED_EDGE('',*,*,#1370,.F.);
#1913=ORIENTED_EDGE('',*,*,#1320,.F.);
#1914=ORIENTED_EDGE('',*,*,#1417,.T.);
#1915=ORIENTED_EDGE('',*,*,#1392,.F.);
#1916=ORIENTED_EDGE('',*,*,#1319,.F.);
#1917=ORIENTED_EDGE('',*,*,#1416,.T.);
#1918=ORIENTED_EDGE('',*,*,#1393,.F.);
#1919=ORIENTED_EDGE('',*,*,#1417,.F.);
#1920=ORIENTED_EDGE('',*,*,#1418,.F.);
#1921=ORIENTED_EDGE('',*,*,#1419,.T.);
#1922=ORIENTED_EDGE('',*,*,#1420,.F.);
#1923=ORIENTED_EDGE('',*,*,#1421,.T.);
#1924=ORIENTED_EDGE('',*,*,#1422,.F.);
#1925=ORIENTED_EDGE('',*,*,#1421,.F.);
#1926=ORIENTED_EDGE('',*,*,#1423,.F.);
#1927=ORIENTED_EDGE('',*,*,#1424,.F.);
#1928=ORIENTED_EDGE('',*,*,#1425,.F.);
#1929=ORIENTED_EDGE('',*,*,#1424,.T.);
#1930=ORIENTED_EDGE('',*,*,#1426,.T.);
#1931=ORIENTED_EDGE('',*,*,#1427,.T.);
#1932=ORIENTED_EDGE('',*,*,#1423,.T.);
#1933=ORIENTED_EDGE('',*,*,#1420,.T.);
#1934=ORIENTED_EDGE('',*,*,#1428,.T.);
#1935=ORIENTED_EDGE('',*,*,#1426,.F.);
#1936=ORIENTED_EDGE('',*,*,#1429,.F.);
#1937=ORIENTED_EDGE('',*,*,#1427,.F.);
#1938=ORIENTED_EDGE('',*,*,#1428,.F.);
#1939=ORIENTED_EDGE('',*,*,#1419,.F.);
#1940=ORIENTED_EDGE('',*,*,#1430,.T.);
#1941=ORIENTED_EDGE('',*,*,#1431,.T.);
#1942=ORIENTED_EDGE('',*,*,#1432,.F.);
#1943=ORIENTED_EDGE('',*,*,#1431,.F.);
#1944=ORIENTED_EDGE('',*,*,#1433,.F.);
#1945=ORIENTED_EDGE('',*,*,#1430,.F.);
#1946=ORIENTED_EDGE('',*,*,#1434,.F.);
#1947=ORIENTED_EDGE('',*,*,#1432,.T.);
#1948=ORIENTED_EDGE('',*,*,#1435,.F.);
#1949=ORIENTED_EDGE('',*,*,#1436,.T.);
#1950=ORIENTED_EDGE('',*,*,#1434,.T.);
#1951=ORIENTED_EDGE('',*,*,#1436,.F.);
#1952=ORIENTED_EDGE('',*,*,#1437,.T.);
#1953=ORIENTED_EDGE('',*,*,#1438,.F.);
#1954=ORIENTED_EDGE('',*,*,#1437,.F.);
#1955=ORIENTED_EDGE('',*,*,#1439,.T.);
#1956=ORIENTED_EDGE('',*,*,#1440,.T.);
#1957=ORIENTED_EDGE('',*,*,#1439,.F.);
#1958=ORIENTED_EDGE('',*,*,#1440,.F.);
#1959=ORIENTED_EDGE('',*,*,#1433,.T.);
#1960=ORIENTED_EDGE('',*,*,#1441,.T.);
#1961=ORIENTED_EDGE('',*,*,#1438,.T.);
#1962=ORIENTED_EDGE('',*,*,#1441,.F.);
#1963=ORIENTED_EDGE('',*,*,#1425,.T.);
#1964=ORIENTED_EDGE('',*,*,#1429,.T.);
#1965=ORIENTED_EDGE('',*,*,#1418,.T.);
#1966=ORIENTED_EDGE('',*,*,#1422,.T.);
#1967=ORIENTED_EDGE('',*,*,#1435,.T.);
#1968=ORIENTED_EDGE('',*,*,#1442,.T.);
#1969=ORIENTED_EDGE('',*,*,#1443,.T.);
#1970=ORIENTED_EDGE('',*,*,#1444,.F.);
#1971=ORIENTED_EDGE('',*,*,#1445,.F.);
#1972=ORIENTED_EDGE('',*,*,#1446,.T.);
#1973=ORIENTED_EDGE('',*,*,#1445,.T.);
#1974=ORIENTED_EDGE('',*,*,#1447,.F.);
#1975=ORIENTED_EDGE('',*,*,#1448,.F.);
#1976=ORIENTED_EDGE('',*,*,#1449,.T.);
#1977=ORIENTED_EDGE('',*,*,#1448,.T.);
#1978=ORIENTED_EDGE('',*,*,#1450,.F.);
#1979=ORIENTED_EDGE('',*,*,#1451,.F.);
#1980=ORIENTED_EDGE('',*,*,#1452,.T.);
#1981=ORIENTED_EDGE('',*,*,#1451,.T.);
#1982=ORIENTED_EDGE('',*,*,#1453,.F.);
#1983=ORIENTED_EDGE('',*,*,#1443,.F.);
#1984=ORIENTED_EDGE('',*,*,#1453,.T.);
#1985=ORIENTED_EDGE('',*,*,#1450,.T.);
#1986=ORIENTED_EDGE('',*,*,#1447,.T.);
#1987=ORIENTED_EDGE('',*,*,#1444,.T.);
#1988=ORIENTED_EDGE('',*,*,#1452,.F.);
#1989=ORIENTED_EDGE('',*,*,#1442,.F.);
#1990=ORIENTED_EDGE('',*,*,#1446,.F.);
#1991=ORIENTED_EDGE('',*,*,#1449,.F.);
#1992=ORIENTED_EDGE('',*,*,#1454,.T.);
#1993=ORIENTED_EDGE('',*,*,#1455,.F.);
#1994=ORIENTED_EDGE('',*,*,#1456,.F.);
#1995=ORIENTED_EDGE('',*,*,#1457,.F.);
#1996=ORIENTED_EDGE('',*,*,#1454,.F.);
#1997=ORIENTED_EDGE('',*,*,#1458,.T.);
#1998=ORIENTED_EDGE('',*,*,#1456,.T.);
#1999=ORIENTED_EDGE('',*,*,#1458,.F.);
#2000=ORIENTED_EDGE('',*,*,#1457,.T.);
#2001=ORIENTED_EDGE('',*,*,#1459,.T.);
#2002=ORIENTED_EDGE('',*,*,#1460,.T.);
#2003=ORIENTED_EDGE('',*,*,#1459,.F.);
#2004=ORIENTED_EDGE('',*,*,#1461,.T.);
#2005=ORIENTED_EDGE('',*,*,#1462,.T.);
#2006=ORIENTED_EDGE('',*,*,#1463,.F.);
#2007=ORIENTED_EDGE('',*,*,#1462,.F.);
#2008=ORIENTED_EDGE('',*,*,#1464,.F.);
#2009=ORIENTED_EDGE('',*,*,#1461,.F.);
#2010=ORIENTED_EDGE('',*,*,#1465,.F.);
#2011=ORIENTED_EDGE('',*,*,#1463,.T.);
#2012=ORIENTED_EDGE('',*,*,#1466,.F.);
#2013=ORIENTED_EDGE('',*,*,#1467,.T.);
#2014=ORIENTED_EDGE('',*,*,#1465,.T.);
#2015=ORIENTED_EDGE('',*,*,#1467,.F.);
#2016=ORIENTED_EDGE('',*,*,#1468,.T.);
#2017=ORIENTED_EDGE('',*,*,#1460,.F.);
#2018=ORIENTED_EDGE('',*,*,#1468,.F.);
#2019=ORIENTED_EDGE('',*,*,#1469,.T.);
#2020=ORIENTED_EDGE('',*,*,#1470,.T.);
#2021=ORIENTED_EDGE('',*,*,#1469,.F.);
#2022=ORIENTED_EDGE('',*,*,#1470,.F.);
#2023=ORIENTED_EDGE('',*,*,#1464,.T.);
#2024=ORIENTED_EDGE('',*,*,#1471,.T.);
#2025=ORIENTED_EDGE('',*,*,#1455,.T.);
#2026=ORIENTED_EDGE('',*,*,#1471,.F.);
#2027=ORIENTED_EDGE('',*,*,#1466,.T.);
#2028=ORIENTED_EDGE('',*,*,#1472,.F.);
#2029=ORIENTED_EDGE('',*,*,#1473,.T.);
#2030=ORIENTED_EDGE('',*,*,#1474,.T.);
#2031=ORIENTED_EDGE('',*,*,#1473,.F.);
#2032=ORIENTED_EDGE('',*,*,#1475,.F.);
#2033=ORIENTED_EDGE('',*,*,#1476,.T.);
#2034=ORIENTED_EDGE('',*,*,#1477,.T.);
#2035=ORIENTED_EDGE('',*,*,#1476,.F.);
#2036=ORIENTED_EDGE('',*,*,#1475,.T.);
#2037=ORIENTED_EDGE('',*,*,#1472,.T.);
#2038=ORIENTED_EDGE('',*,*,#1477,.F.);
#2039=ORIENTED_EDGE('',*,*,#1474,.F.);
#2040=ORIENTED_EDGE('',*,*,#1478,.F.);
#2041=ORIENTED_EDGE('',*,*,#1479,.T.);
#2042=ORIENTED_EDGE('',*,*,#1480,.T.);
#2043=ORIENTED_EDGE('',*,*,#1479,.F.);
#2044=ORIENTED_EDGE('',*,*,#1481,.F.);
#2045=ORIENTED_EDGE('',*,*,#1482,.T.);
#2046=ORIENTED_EDGE('',*,*,#1483,.T.);
#2047=ORIENTED_EDGE('',*,*,#1482,.F.);
#2048=ORIENTED_EDGE('',*,*,#1481,.T.);
#2049=ORIENTED_EDGE('',*,*,#1478,.T.);
#2050=ORIENTED_EDGE('',*,*,#1483,.F.);
#2051=ORIENTED_EDGE('',*,*,#1480,.F.);
#2052=ORIENTED_EDGE('',*,*,#1484,.F.);
#2053=ORIENTED_EDGE('',*,*,#1485,.T.);
#2054=ORIENTED_EDGE('',*,*,#1486,.T.);
#2055=ORIENTED_EDGE('',*,*,#1485,.F.);
#2056=ORIENTED_EDGE('',*,*,#1487,.F.);
#2057=ORIENTED_EDGE('',*,*,#1488,.T.);
#2058=ORIENTED_EDGE('',*,*,#1489,.T.);
#2059=ORIENTED_EDGE('',*,*,#1488,.F.);
#2060=ORIENTED_EDGE('',*,*,#1487,.T.);
#2061=ORIENTED_EDGE('',*,*,#1484,.T.);
#2062=ORIENTED_EDGE('',*,*,#1489,.F.);
#2063=ORIENTED_EDGE('',*,*,#1486,.F.);
#2064=ORIENTED_EDGE('',*,*,#1490,.F.);
#2065=ORIENTED_EDGE('',*,*,#1491,.T.);
#2066=ORIENTED_EDGE('',*,*,#1492,.T.);
#2067=ORIENTED_EDGE('',*,*,#1491,.F.);
#2068=ORIENTED_EDGE('',*,*,#1493,.F.);
#2069=ORIENTED_EDGE('',*,*,#1494,.T.);
#2070=ORIENTED_EDGE('',*,*,#1495,.T.);
#2071=ORIENTED_EDGE('',*,*,#1494,.F.);
#2072=ORIENTED_EDGE('',*,*,#1493,.T.);
#2073=ORIENTED_EDGE('',*,*,#1490,.T.);
#2074=ORIENTED_EDGE('',*,*,#1495,.F.);
#2075=ORIENTED_EDGE('',*,*,#1492,.F.);
#2076=ORIENTED_EDGE('',*,*,#1496,.F.);
#2077=ORIENTED_EDGE('',*,*,#1497,.F.);
#2078=ORIENTED_EDGE('',*,*,#1498,.F.);
#2079=ORIENTED_EDGE('',*,*,#1499,.F.);
#2080=ORIENTED_EDGE('',*,*,#1500,.F.);
#2081=ORIENTED_EDGE('',*,*,#1501,.F.);
#2082=ORIENTED_EDGE('',*,*,#1502,.F.);
#2083=ORIENTED_EDGE('',*,*,#1503,.F.);
#2084=ORIENTED_EDGE('',*,*,#1503,.T.);
#2085=ORIENTED_EDGE('',*,*,#1504,.F.);
#2086=ORIENTED_EDGE('',*,*,#1497,.T.);
#2087=ORIENTED_EDGE('',*,*,#1505,.F.);
#2088=ORIENTED_EDGE('',*,*,#1500,.T.);
#2089=ORIENTED_EDGE('',*,*,#1505,.T.);
#2090=ORIENTED_EDGE('',*,*,#1496,.T.);
#2091=ORIENTED_EDGE('',*,*,#1506,.F.);
#2092=ORIENTED_EDGE('',*,*,#1502,.T.);
#2093=ORIENTED_EDGE('',*,*,#1507,.F.);
#2094=ORIENTED_EDGE('',*,*,#1498,.T.);
#2095=ORIENTED_EDGE('',*,*,#1504,.T.);
#2096=ORIENTED_EDGE('',*,*,#1501,.T.);
#2097=ORIENTED_EDGE('',*,*,#1506,.T.);
#2098=ORIENTED_EDGE('',*,*,#1499,.T.);
#2099=ORIENTED_EDGE('',*,*,#1507,.T.);
#2100=CYLINDRICAL_SURFACE('',#2430,4.5);
#2101=CYLINDRICAL_SURFACE('',#2433,4.5);
#2102=CYLINDRICAL_SURFACE('',#2436,4.5);
#2103=CYLINDRICAL_SURFACE('',#2439,4.5);
#2104=CYLINDRICAL_SURFACE('',#2442,7.);
#2105=CYLINDRICAL_SURFACE('',#2445,7.);
#2106=CYLINDRICAL_SURFACE('',#2462,4.);
#2107=CYLINDRICAL_SURFACE('',#2469,5.);
#2108=CYLINDRICAL_SURFACE('',#2471,5.);
#2109=CYLINDRICAL_SURFACE('',#2488,40.);
#2110=CYLINDRICAL_SURFACE('',#2489,12.);
#2111=CYLINDRICAL_SURFACE('',#2495,65.);
#2112=CYLINDRICAL_SURFACE('',#2496,5.);
#2113=CYLINDRICAL_SURFACE('',#2498,5.);
#2114=CYLINDRICAL_SURFACE('',#2506,5.);
#2115=CYLINDRICAL_SURFACE('',#2534,41.);
#2116=CYLINDRICAL_SURFACE('',#2536,41.);
#2117=CYLINDRICAL_SURFACE('',#2538,41.);
#2118=CYLINDRICAL_SURFACE('',#2540,41.);
#2119=CYLINDRICAL_SURFACE('',#2542,41.);
#2120=CYLINDRICAL_SURFACE('',#2544,41.);
#2121=CYLINDRICAL_SURFACE('',#2546,90.);
#2122=CYLINDRICAL_SURFACE('',#2548,90.);
#2123=CYLINDRICAL_SURFACE('',#2550,90.);
#2124=CYLINDRICAL_SURFACE('',#2552,90.);
#2125=CYLINDRICAL_SURFACE('',#2554,90.);
#2126=CYLINDRICAL_SURFACE('',#2556,90.);
#2127=CYLINDRICAL_SURFACE('',#2571,90.);
#2128=CYLINDRICAL_SURFACE('',#2572,90.);
#2129=CYLINDRICAL_SURFACE('',#2575,6.);
#2130=CYLINDRICAL_SURFACE('',#2578,6.);
#2131=CYLINDRICAL_SURFACE('',#2581,6.);
#2132=CYLINDRICAL_SURFACE('',#2582,90.);
#2133=CYLINDRICAL_SURFACE('',#2583,90.);
#2134=CYLINDRICAL_SURFACE('',#2586,6.);
#2135=CYLINDRICAL_SURFACE('',#2589,6.);
#2136=CYLINDRICAL_SURFACE('',#2590,90.);
#2137=CYLINDRICAL_SURFACE('',#2591,90.);
#2138=CYLINDRICAL_SURFACE('',#2594,6.);
#2139=CYLINDRICAL_SURFACE('',#2603,4.);
#2140=CYLINDRICAL_SURFACE('',#2610,5.);
#2141=CYLINDRICAL_SURFACE('',#2615,8.);
#2142=CYLINDRICAL_SURFACE('',#2618,5.);
#2143=CYLINDRICAL_SURFACE('',#2634,7.);
#2144=CYLINDRICAL_SURFACE('',#2635,5.);
#2145=CYLINDRICAL_SURFACE('',#2637,4.);
#2146=CYLINDRICAL_SURFACE('',#2644,5.);
#2147=CYLINDRICAL_SURFACE('',#2648,8.);
#2148=CYLINDRICAL_SURFACE('',#2651,5.);
#2149=CYLINDRICAL_SURFACE('',#2654,5.);
#2150=CYLINDRICAL_SURFACE('',#2657,7.);
#2151=CYLINDRICAL_SURFACE('',#2663,5.);
#2152=CYLINDRICAL_SURFACE('',#2666,7.);
#2153=CYLINDRICAL_SURFACE('',#2672,5.);
#2154=CYLINDRICAL_SURFACE('',#2675,7.);
#2155=CYLINDRICAL_SURFACE('',#2681,5.);
#2156=CYLINDRICAL_SURFACE('',#2684,10.);
#2157=CYLINDRICAL_SURFACE('',#2695,4.);
#2158=CYLINDRICAL_SURFACE('',#2697,8.);
#2159=ADVANCED_FACE('',(#238),#2100,.F.);
#2160=ADVANCED_FACE('',(#239),#2101,.F.);
#2161=ADVANCED_FACE('',(#240),#2102,.F.);
#2162=ADVANCED_FACE('',(#241),#2103,.F.);
#2163=ADVANCED_FACE('',(#242),#2104,.F.);
#2164=ADVANCED_FACE('',(#243),#2105,.F.);
#2165=ADVANCED_FACE('',(#244),#161,.T.);
#2166=ADVANCED_FACE('',(#245),#162,.T.);
#2167=ADVANCED_FACE('',(#246),#163,.T.);
#2168=ADVANCED_FACE('',(#247),#164,.T.);
#2169=ADVANCED_FACE('',(#248,#123,#124,#125,#126,#127,#128),#165,.T.);
#2170=ADVANCED_FACE('',(#249,#129,#130,#131,#132,#133,#134),#166,.F.);
#2171=ADVANCED_FACE('',(#250),#167,.T.);
#2172=ADVANCED_FACE('',(#251),#168,.T.);
#2173=ADVANCED_FACE('',(#252),#169,.T.);
#2174=ADVANCED_FACE('',(#253),#170,.T.);
#2175=ADVANCED_FACE('',(#254),#171,.T.);
#2176=ADVANCED_FACE('',(#255),#172,.T.);
#2177=ADVANCED_FACE('',(#256),#173,.T.);
#2178=ADVANCED_FACE('',(#257),#2106,.T.);
#2179=ADVANCED_FACE('',(#258,#135),#174,.F.);
#2180=ADVANCED_FACE('',(#259,#136),#175,.F.);
#2181=ADVANCED_FACE('',(#260),#2107,.T.);
#2182=ADVANCED_FACE('',(#261),#2108,.F.);
#2183=ADVANCED_FACE('',(#262),#176,.F.);
#2184=ADVANCED_FACE('',(#263),#177,.F.);
#2185=ADVANCED_FACE('',(#264),#178,.F.);
#2186=ADVANCED_FACE('',(#265),#179,.F.);
#2187=ADVANCED_FACE('',(#266),#180,.T.);
#2188=ADVANCED_FACE('',(#267),#181,.F.);
#2189=ADVANCED_FACE('',(#268),#2109,.T.);
#2190=ADVANCED_FACE('',(#269),#2110,.T.);
#2191=ADVANCED_FACE('',(#270,#137,#138),#182,.T.);
#2192=ADVANCED_FACE('',(#271,#139,#140),#183,.F.);
#2193=ADVANCED_FACE('',(#272),#2111,.T.);
#2194=ADVANCED_FACE('',(#273),#2112,.T.);
#2195=ADVANCED_FACE('',(#274),#2113,.T.);
#2196=ADVANCED_FACE('',(#275,#141),#184,.T.);
#2197=ADVANCED_FACE('',(#276),#185,.F.);
#2198=ADVANCED_FACE('',(#277),#186,.F.);
#2199=ADVANCED_FACE('',(#278),#187,.F.);
#2200=ADVANCED_FACE('',(#279),#188,.F.);
#2201=ADVANCED_FACE('',(#280),#2114,.F.);
#2202=ADVANCED_FACE('',(#281,#142),#189,.T.);
#2203=ADVANCED_FACE('',(#282),#2115,.F.);
#2204=ADVANCED_FACE('',(#283),#2116,.F.);
#2205=ADVANCED_FACE('',(#284),#2117,.F.);
#2206=ADVANCED_FACE('',(#285),#2118,.F.);
#2207=ADVANCED_FACE('',(#286),#2119,.F.);
#2208=ADVANCED_FACE('',(#287),#2120,.F.);
#2209=ADVANCED_FACE('',(#288),#2121,.T.);
#2210=ADVANCED_FACE('',(#289),#2122,.T.);
#2211=ADVANCED_FACE('',(#290),#2123,.T.);
#2212=ADVANCED_FACE('',(#291),#2124,.T.);
#2213=ADVANCED_FACE('',(#292),#2125,.T.);
#2214=ADVANCED_FACE('',(#293),#2126,.T.);
#2215=ADVANCED_FACE('',(#294,#143),#190,.F.);
#2216=ADVANCED_FACE('',(#295),#2127,.T.);
#2217=ADVANCED_FACE('',(#296),#2128,.T.);
#2218=ADVANCED_FACE('',(#297),#191,.F.);
#2219=ADVANCED_FACE('',(#298),#192,.F.);
#2220=ADVANCED_FACE('',(#299),#2129,.F.);
#2221=ADVANCED_FACE('',(#300),#193,.F.);
#2222=ADVANCED_FACE('',(#301),#194,.F.);
#2223=ADVANCED_FACE('',(#302),#2130,.F.);
#2224=ADVANCED_FACE('',(#303),#195,.F.);
#2225=ADVANCED_FACE('',(#304),#196,.F.);
#2226=ADVANCED_FACE('',(#305),#2131,.F.);
#2227=ADVANCED_FACE('',(#306),#2132,.T.);
#2228=ADVANCED_FACE('',(#307),#2133,.T.);
#2229=ADVANCED_FACE('',(#308),#197,.F.);
#2230=ADVANCED_FACE('',(#309),#198,.F.);
#2231=ADVANCED_FACE('',(#310),#2134,.F.);
#2232=ADVANCED_FACE('',(#311),#199,.F.);
#2233=ADVANCED_FACE('',(#312),#200,.F.);
#2234=ADVANCED_FACE('',(#313),#2135,.F.);
#2235=ADVANCED_FACE('',(#314),#2136,.T.);
#2236=ADVANCED_FACE('',(#315),#2137,.T.);
#2237=ADVANCED_FACE('',(#316),#201,.F.);
#2238=ADVANCED_FACE('',(#317),#202,.F.);
#2239=ADVANCED_FACE('',(#318),#2138,.F.);
#2240=ADVANCED_FACE('',(#319),#203,.F.);
#2241=ADVANCED_FACE('',(#320),#204,.F.);
#2242=ADVANCED_FACE('',(#321),#205,.F.);
#2243=ADVANCED_FACE('',(#322),#206,.F.);
#2244=ADVANCED_FACE('',(#323),#207,.F.);
#2245=ADVANCED_FACE('',(#324),#2139,.T.);
#2246=ADVANCED_FACE('',(#325,#144),#208,.F.);
#2247=ADVANCED_FACE('',(#326,#145),#209,.F.);
#2248=ADVANCED_FACE('',(#327),#2140,.T.);
#2249=ADVANCED_FACE('',(#328,#146),#210,.T.);
#2250=ADVANCED_FACE('',(#329),#2141,.T.);
#2251=ADVANCED_FACE('',(#330),#211,.F.);
#2252=ADVANCED_FACE('',(#331,#147),#2142,.T.);
#2253=ADVANCED_FACE('',(#332),#212,.T.);
#2254=ADVANCED_FACE('',(#333),#213,.T.);
#2255=ADVANCED_FACE('',(#334),#214,.T.);
#2256=ADVANCED_FACE('',(#335),#215,.T.);
#2257=ADVANCED_FACE('',(#336),#216,.T.);
#2258=ADVANCED_FACE('',(#337),#217,.T.);
#2259=ADVANCED_FACE('',(#338),#218,.F.);
#2260=ADVANCED_FACE('',(#339,#148),#219,.T.);
#2261=ADVANCED_FACE('',(#340,#149),#220,.F.);
#2262=ADVANCED_FACE('',(#341),#2143,.T.);
#2263=ADVANCED_FACE('',(#342),#2144,.T.);
#2264=ADVANCED_FACE('',(#343),#2145,.T.);
#2265=ADVANCED_FACE('',(#344,#150),#221,.F.);
#2266=ADVANCED_FACE('',(#345,#151),#222,.F.);
#2267=ADVANCED_FACE('',(#346),#2146,.T.);
#2268=ADVANCED_FACE('',(#347,#152),#223,.T.);
#2269=ADVANCED_FACE('',(#348),#2147,.T.);
#2270=ADVANCED_FACE('',(#349),#224,.F.);
#2271=ADVANCED_FACE('',(#350),#2148,.T.);
#2272=ADVANCED_FACE('',(#351),#225,.T.);
#2273=ADVANCED_FACE('',(#352),#2149,.F.);
#2274=ADVANCED_FACE('',(#353),#2150,.T.);
#2275=ADVANCED_FACE('',(#354,#153),#226,.T.);
#2276=ADVANCED_FACE('',(#355,#154),#227,.F.);
#2277=ADVANCED_FACE('',(#356),#2151,.F.);
#2278=ADVANCED_FACE('',(#357),#2152,.T.);
#2279=ADVANCED_FACE('',(#358,#155),#228,.T.);
#2280=ADVANCED_FACE('',(#359,#156),#229,.F.);
#2281=ADVANCED_FACE('',(#360),#2153,.F.);
#2282=ADVANCED_FACE('',(#361),#2154,.T.);
#2283=ADVANCED_FACE('',(#362,#157),#230,.T.);
#2284=ADVANCED_FACE('',(#363,#158),#231,.F.);
#2285=ADVANCED_FACE('',(#364),#2155,.F.);
#2286=ADVANCED_FACE('',(#365),#2156,.T.);
#2287=ADVANCED_FACE('',(#366,#159),#232,.T.);
#2288=ADVANCED_FACE('',(#367,#160),#233,.F.);
#2289=ADVANCED_FACE('',(#368),#234,.F.);
#2290=ADVANCED_FACE('',(#369),#235,.F.);
#2291=ADVANCED_FACE('',(#370),#236,.F.);
#2292=ADVANCED_FACE('',(#371),#2157,.F.);
#2293=ADVANCED_FACE('',(#372),#2158,.T.);
#2294=ADVANCED_FACE('',(#373),#237,.T.);
#2295=CLOSED_SHELL('',(#2159,#2160,#2161,#2162,#2163,#2164,#2165,#2166,
#2167,#2168,#2169,#2170));
#2296=CLOSED_SHELL('',(#2171,#2172,#2173,#2174,#2175,#2176,#2177,#2178,
#2179,#2180,#2181,#2182,#2183,#2184,#2185,#2186,#2187,#2188,#2189,#2190,
#2191,#2192,#2193,#2194,#2195,#2196,#2197));
#2297=CLOSED_SHELL('',(#2198,#2199,#2200,#2201,#2202,#2203,#2204,#2205,
#2206,#2207,#2208,#2209,#2210,#2211,#2212,#2213,#2214,#2215,#2216,#2217,
#2218,#2219,#2220,#2221,#2222,#2223,#2224,#2225,#2226,#2227,#2228,#2229,
#2230,#2231,#2232,#2233,#2234,#2235,#2236,#2237,#2238,#2239));
#2298=CLOSED_SHELL('',(#2240,#2241,#2242,#2243,#2244,#2245,#2246,#2247,
#2248,#2249,#2250,#2251,#2252,#2253));
#2299=CLOSED_SHELL('',(#2254,#2255,#2256,#2257,#2258,#2259));
#2300=CLOSED_SHELL('',(#2260,#2261,#2262,#2263,#2264,#2265,#2266,#2267,
#2268,#2269,#2270,#2271,#2272));
#2301=CLOSED_SHELL('',(#2273,#2274,#2275,#2276));
#2302=CLOSED_SHELL('',(#2277,#2278,#2279,#2280));
#2303=CLOSED_SHELL('',(#2281,#2282,#2283,#2284));
#2304=CLOSED_SHELL('',(#2285,#2286,#2287,#2288));
#2305=CLOSED_SHELL('',(#2289,#2290,#2291,#2292,#2293,#2294));
#2306=DERIVED_UNIT_ELEMENT(#2328,1.);
#2307=DERIVED_UNIT_ELEMENT(#4151,-3.);
#2308=DERIVED_UNIT_ELEMENT(#2328,1.);
#2309=DERIVED_UNIT_ELEMENT(#4151,-3.);
#2310=DERIVED_UNIT_ELEMENT(#2328,1.);
#2311=DERIVED_UNIT_ELEMENT(#4151,-3.);
#2312=DERIVED_UNIT_ELEMENT(#2328,1.);
#2313=DERIVED_UNIT_ELEMENT(#4151,-3.);
#2314=DERIVED_UNIT_ELEMENT(#2328,1.);
#2315=DERIVED_UNIT_ELEMENT(#4151,-3.);
#2316=DERIVED_UNIT_ELEMENT(#2328,1.);
#2317=DERIVED_UNIT_ELEMENT(#4151,-3.);
#2318=DERIVED_UNIT_ELEMENT(#2328,1.);
#2319=DERIVED_UNIT_ELEMENT(#4151,-3.);
#2320=DERIVED_UNIT_ELEMENT(#2328,1.);
#2321=DERIVED_UNIT_ELEMENT(#4151,-3.);
#2322=DERIVED_UNIT_ELEMENT(#2328,1.);
#2323=DERIVED_UNIT_ELEMENT(#4151,-3.);
#2324=DERIVED_UNIT_ELEMENT(#2328,1.);
#2325=DERIVED_UNIT_ELEMENT(#4151,-3.);
#2326=DERIVED_UNIT_ELEMENT(#2328,1.);
#2327=DERIVED_UNIT_ELEMENT(#4151,-3.);
#2328=(
MASS_UNIT()
NAMED_UNIT(*)
SI_UNIT(.KILO.,.GRAM.)
);
#2329=DERIVED_UNIT((#2306,#2307));
#2330=DERIVED_UNIT((#2308,#2309));
#2331=DERIVED_UNIT((#2310,#2311));
#2332=DERIVED_UNIT((#2312,#2313));
#2333=DERIVED_UNIT((#2314,#2315));
#2334=DERIVED_UNIT((#2316,#2317));
#2335=DERIVED_UNIT((#2318,#2319));
#2336=DERIVED_UNIT((#2320,#2321));
#2337=DERIVED_UNIT((#2322,#2323));
#2338=DERIVED_UNIT((#2324,#2325));
#2339=DERIVED_UNIT((#2326,#2327));
#2340=MEASURE_REPRESENTATION_ITEM('density measure',
POSITIVE_RATIO_MEASURE(7850.),#2329);
#2341=MEASURE_REPRESENTATION_ITEM('density measure',
POSITIVE_RATIO_MEASURE(7850.),#2330);
#2342=MEASURE_REPRESENTATION_ITEM('density measure',
POSITIVE_RATIO_MEASURE(7850.),#2331);
#2343=MEASURE_REPRESENTATION_ITEM('density measure',
POSITIVE_RATIO_MEASURE(7850.),#2332);
#2344=MEASURE_REPRESENTATION_ITEM('density measure',
POSITIVE_RATIO_MEASURE(7850.),#2333);
#2345=MEASURE_REPRESENTATION_ITEM('density measure',
POSITIVE_RATIO_MEASURE(7850.),#2334);
#2346=MEASURE_REPRESENTATION_ITEM('density measure',
POSITIVE_RATIO_MEASURE(8920.),#2335);
#2347=MEASURE_REPRESENTATION_ITEM('density measure',
POSITIVE_RATIO_MEASURE(7850.),#2336);
#2348=MEASURE_REPRESENTATION_ITEM('density measure',
POSITIVE_RATIO_MEASURE(7850.),#2337);
#2349=MEASURE_REPRESENTATION_ITEM('density measure',
POSITIVE_RATIO_MEASURE(7850.),#2338);
#2350=MEASURE_REPRESENTATION_ITEM('density measure',
POSITIVE_RATIO_MEASURE(7850.),#2339);
#2351=PROPERTY_DEFINITION_REPRESENTATION(#2406,#2373);
#2352=PROPERTY_DEFINITION_REPRESENTATION(#2407,#2374);
#2353=PROPERTY_DEFINITION_REPRESENTATION(#2408,#2375);
#2354=PROPERTY_DEFINITION_REPRESENTATION(#2409,#2376);
#2355=PROPERTY_DEFINITION_REPRESENTATION(#2410,#2377);
#2356=PROPERTY_DEFINITION_REPRESENTATION(#2411,#2378);
#2357=PROPERTY_DEFINITION_REPRESENTATION(#2412,#2379);
#2358=PROPERTY_DEFINITION_REPRESENTATION(#2413,#2380);
#2359=PROPERTY_DEFINITION_REPRESENTATION(#2414,#2381);
#2360=PROPERTY_DEFINITION_REPRESENTATION(#2415,#2382);
#2361=PROPERTY_DEFINITION_REPRESENTATION(#2416,#2383);
#2362=PROPERTY_DEFINITION_REPRESENTATION(#2417,#2384);
#2363=PROPERTY_DEFINITION_REPRESENTATION(#2418,#2385);
#2364=PROPERTY_DEFINITION_REPRESENTATION(#2419,#2386);
#2365=PROPERTY_DEFINITION_REPRESENTATION(#2420,#2387);
#2366=PROPERTY_DEFINITION_REPRESENTATION(#2421,#2388);
#2367=PROPERTY_DEFINITION_REPRESENTATION(#2422,#2389);
#2368=PROPERTY_DEFINITION_REPRESENTATION(#2423,#2390);
#2369=PROPERTY_DEFINITION_REPRESENTATION(#2424,#2391);
#2370=PROPERTY_DEFINITION_REPRESENTATION(#2425,#2392);
#2371=PROPERTY_DEFINITION_REPRESENTATION(#2426,#2393);
#2372=PROPERTY_DEFINITION_REPRESENTATION(#2427,#2394);
#2373=REPRESENTATION('material name',(#2395),#4138);
#2374=REPRESENTATION('density',(#2340),#4138);
#2375=REPRESENTATION('material name',(#2396),#4139);
#2376=REPRESENTATION('density',(#2341),#4139);
#2377=REPRESENTATION('material name',(#2397),#4140);
#2378=REPRESENTATION('density',(#2342),#4140);
#2379=REPRESENTATION('material name',(#2398),#4141);
#2380=REPRESENTATION('density',(#2343),#4141);
#2381=REPRESENTATION('material name',(#2399),#4142);
#2382=REPRESENTATION('density',(#2344),#4142);
#2383=REPRESENTATION('material name',(#2400),#4143);
#2384=REPRESENTATION('density',(#2345),#4143);
#2385=REPRESENTATION('material name',(#2401),#4144);
#2386=REPRESENTATION('density',(#2346),#4144);
#2387=REPRESENTATION('material name',(#2402),#4145);
#2388=REPRESENTATION('density',(#2347),#4145);
#2389=REPRESENTATION('material name',(#2403),#4146);
#2390=REPRESENTATION('density',(#2348),#4146);
#2391=REPRESENTATION('material name',(#2404),#4147);
#2392=REPRESENTATION('density',(#2349),#4147);
#2393=REPRESENTATION('material name',(#2405),#4148);
#2394=REPRESENTATION('density',(#2350),#4148);
#2395=DESCRIPTIVE_REPRESENTATION_ITEM('Steel','Steel');
#2396=DESCRIPTIVE_REPRESENTATION_ITEM('Steel','Steel');
#2397=DESCRIPTIVE_REPRESENTATION_ITEM('Steel','Steel');
#2398=DESCRIPTIVE_REPRESENTATION_ITEM('Steel','Steel');
#2399=DESCRIPTIVE_REPRESENTATION_ITEM('Steel','Steel');
#2400=DESCRIPTIVE_REPRESENTATION_ITEM('Steel','Steel');
#2401=DESCRIPTIVE_REPRESENTATION_ITEM('Copper, Alloy','Copper, Alloy');
#2402=DESCRIPTIVE_REPRESENTATION_ITEM('Steel','Steel');
#2403=DESCRIPTIVE_REPRESENTATION_ITEM('Steel','Steel');
#2404=DESCRIPTIVE_REPRESENTATION_ITEM('Steel','Steel');
#2405=DESCRIPTIVE_REPRESENTATION_ITEM('Steel','Steel');
#2406=PROPERTY_DEFINITION('material property','material name',#4209);
#2407=PROPERTY_DEFINITION('material property','density of part',#4209);
#2408=PROPERTY_DEFINITION('material property','material name',#4210);
#2409=PROPERTY_DEFINITION('material property','density of part',#4210);
#2410=PROPERTY_DEFINITION('material property','material name',#4211);
#2411=PROPERTY_DEFINITION('material property','density of part',#4211);
#2412=PROPERTY_DEFINITION('material property','material name',#4212);
#2413=PROPERTY_DEFINITION('material property','density of part',#4212);
#2414=PROPERTY_DEFINITION('material property','material name',#4213);
#2415=PROPERTY_DEFINITION('material property','density of part',#4213);
#2416=PROPERTY_DEFINITION('material property','material name',#4214);
#2417=PROPERTY_DEFINITION('material property','density of part',#4214);
#2418=PROPERTY_DEFINITION('material property','material name',#4215);
#2419=PROPERTY_DEFINITION('material property','density of part',#4215);
#2420=PROPERTY_DEFINITION('material property','material name',#4216);
#2421=PROPERTY_DEFINITION('material property','density of part',#4216);
#2422=PROPERTY_DEFINITION('material property','material name',#4217);
#2423=PROPERTY_DEFINITION('material property','density of part',#4217);
#2424=PROPERTY_DEFINITION('material property','material name',#4218);
#2425=PROPERTY_DEFINITION('material property','density of part',#4218);
#2426=PROPERTY_DEFINITION('material property','material name',#4219);
#2427=PROPERTY_DEFINITION('material property','density of part',#4219);
#2428=AXIS2_PLACEMENT_3D('',#3467,#2717,#2718);
#2429=AXIS2_PLACEMENT_3D('',#3468,#2719,#2720);
#2430=AXIS2_PLACEMENT_3D('',#3469,#2721,#2722);
#2431=AXIS2_PLACEMENT_3D('',#3471,#2723,#2724);
#2432=AXIS2_PLACEMENT_3D('',#3474,#2726,#2727);
#2433=AXIS2_PLACEMENT_3D('',#3475,#2728,#2729);
#2434=AXIS2_PLACEMENT_3D('',#3477,#2730,#2731);
#2435=AXIS2_PLACEMENT_3D('',#3480,#2733,#2734);
#2436=AXIS2_PLACEMENT_3D('',#3481,#2735,#2736);
#2437=AXIS2_PLACEMENT_3D('',#3483,#2737,#2738);
#2438=AXIS2_PLACEMENT_3D('',#3486,#2740,#2741);
#2439=AXIS2_PLACEMENT_3D('',#3487,#2742,#2743);
#2440=AXIS2_PLACEMENT_3D('',#3489,#2744,#2745);
#2441=AXIS2_PLACEMENT_3D('',#3492,#2747,#2748);
#2442=AXIS2_PLACEMENT_3D('',#3493,#2749,#2750);
#2443=AXIS2_PLACEMENT_3D('',#3495,#2751,#2752);
#2444=AXIS2_PLACEMENT_3D('',#3498,#2754,#2755);
#2445=AXIS2_PLACEMENT_3D('',#3499,#2756,#2757);
#2446=AXIS2_PLACEMENT_3D('',#3501,#2758,#2759);
#2447=AXIS2_PLACEMENT_3D('',#3504,#2761,#2762);
#2448=AXIS2_PLACEMENT_3D('',#3505,#2763,#2764);
#2449=AXIS2_PLACEMENT_3D('',#3514,#2769,#2770);
#2450=AXIS2_PLACEMENT_3D('',#3520,#2774,#2775);
#2451=AXIS2_PLACEMENT_3D('',#3526,#2779,#2780);
#2452=AXIS2_PLACEMENT_3D('',#3529,#2783,#2784);
#2453=AXIS2_PLACEMENT_3D('',#3530,#2785,#2786);
#2454=AXIS2_PLACEMENT_3D('',#3531,#2787,#2788);
#2455=AXIS2_PLACEMENT_3D('',#3532,#2789,#2790);
#2456=AXIS2_PLACEMENT_3D('',#3541,#2795,#2796);
#2457=AXIS2_PLACEMENT_3D('',#3547,#2800,#2801);
#2458=AXIS2_PLACEMENT_3D('',#3553,#2805,#2806);
#2459=AXIS2_PLACEMENT_3D('',#3559,#2810,#2811);
#2460=AXIS2_PLACEMENT_3D('',#3565,#2815,#2816);
#2461=AXIS2_PLACEMENT_3D('',#3568,#2819,#2820);
#2462=AXIS2_PLACEMENT_3D('',#3569,#2821,#2822);
#2463=AXIS2_PLACEMENT_3D('',#3571,#2823,#2824);
#2464=AXIS2_PLACEMENT_3D('',#3574,#2826,#2827);
#2465=AXIS2_PLACEMENT_3D('',#3575,#2828,#2829);
#2466=AXIS2_PLACEMENT_3D('',#3577,#2830,#2831);
#2467=AXIS2_PLACEMENT_3D('',#3578,#2832,#2833);
#2468=AXIS2_PLACEMENT_3D('',#3580,#2834,#2835);
#2469=AXIS2_PLACEMENT_3D('',#3581,#2836,#2837);
#2470=AXIS2_PLACEMENT_3D('',#3583,#2838,#2839);
#2471=AXIS2_PLACEMENT_3D('',#3585,#2841,#2842);
#2472=AXIS2_PLACEMENT_3D('',#3587,#2843,#2844);
#2473=AXIS2_PLACEMENT_3D('',#3590,#2846,#2847);
#2474=AXIS2_PLACEMENT_3D('',#3591,#2848,#2849);
#2475=AXIS2_PLACEMENT_3D('',#3594,#2850,#2851);
#2476=AXIS2_PLACEMENT_3D('',#3598,#2854,#2855);
#2477=AXIS2_PLACEMENT_3D('',#3601,#2856,#2857);
#2478=AXIS2_PLACEMENT_3D('',#3605,#2860,#2861);
#2479=AXIS2_PLACEMENT_3D('',#3612,#2866,#2867);
#2480=AXIS2_PLACEMENT_3D('',#3618,#2871,#2872);
#2481=AXIS2_PLACEMENT_3D('',#3620,#2873,#2874);
#2482=AXIS2_PLACEMENT_3D('',#3621,#2875,#2876);
#2483=AXIS2_PLACEMENT_3D('',#3622,#2877,#2878);
#2484=AXIS2_PLACEMENT_3D('',#3623,#2879,#2880);
#2485=AXIS2_PLACEMENT_3D('',#3624,#2881,#2882);
#2486=AXIS2_PLACEMENT_3D('',#3626,#2883,#2884);
#2487=AXIS2_PLACEMENT_3D('',#3627,#2885,#2886);
#2488=AXIS2_PLACEMENT_3D('',#3628,#2887,#2888);
#2489=AXIS2_PLACEMENT_3D('',#3629,#2889,#2890);
#2490=AXIS2_PLACEMENT_3D('',#3632,#2892,#2893);
#2491=AXIS2_PLACEMENT_3D('',#3633,#2894,#2895);
#2492=AXIS2_PLACEMENT_3D('',#3635,#2896,#2897);
#2493=AXIS2_PLACEMENT_3D('',#3636,#2898,#2899);
#2494=AXIS2_PLACEMENT_3D('',#3638,#2900,#2901);
#2495=AXIS2_PLACEMENT_3D('',#3639,#2902,#2903);
#2496=AXIS2_PLACEMENT_3D('',#3641,#2905,#2906);
#2497=AXIS2_PLACEMENT_3D('',#3644,#2908,#2909);
#2498=AXIS2_PLACEMENT_3D('',#3645,#2910,#2911);
#2499=AXIS2_PLACEMENT_3D('',#3647,#2912,#2913);
#2500=AXIS2_PLACEMENT_3D('',#3649,#2915,#2916);
#2501=AXIS2_PLACEMENT_3D('',#3650,#2917,#2918);
#2502=AXIS2_PLACEMENT_3D('',#3651,#2919,#2920);
#2503=AXIS2_PLACEMENT_3D('',#3652,#2921,#2922);
#2504=AXIS2_PLACEMENT_3D('',#3661,#2927,#2928);
#2505=AXIS2_PLACEMENT_3D('',#3670,#2933,#2934);
#2506=AXIS2_PLACEMENT_3D('',#3673,#2937,#2938);
#2507=AXIS2_PLACEMENT_3D('',#3674,#2939,#2940);
#2508=AXIS2_PLACEMENT_3D('',#3675,#2941,#2942);
#2509=AXIS2_PLACEMENT_3D('',#3676,#2943,#2944);
#2510=AXIS2_PLACEMENT_3D('',#3679,#2945,#2946);
#2511=AXIS2_PLACEMENT_3D('',#3681,#2947,#2948);
#2512=AXIS2_PLACEMENT_3D('',#3685,#2950,#2951);
#2513=AXIS2_PLACEMENT_3D('',#3689,#2953,#2954);
#2514=AXIS2_PLACEMENT_3D('',#3691,#2955,#2956);
#2515=AXIS2_PLACEMENT_3D('',#3693,#2957,#2958);
#2516=AXIS2_PLACEMENT_3D('',#3697,#2960,#2961);
#2517=AXIS2_PLACEMENT_3D('',#3701,#2963,#2964);
#2518=AXIS2_PLACEMENT_3D('',#3703,#2965,#2966);
#2519=AXIS2_PLACEMENT_3D('',#3705,#2967,#2968);
#2520=AXIS2_PLACEMENT_3D('',#3709,#2970,#2971);
#2521=AXIS2_PLACEMENT_3D('',#3713,#2973,#2974);
#2522=AXIS2_PLACEMENT_3D('',#3715,#2975,#2976);
#2523=AXIS2_PLACEMENT_3D('',#3717,#2977,#2978);
#2524=AXIS2_PLACEMENT_3D('',#3721,#2980,#2981);
#2525=AXIS2_PLACEMENT_3D('',#3725,#2983,#2984);
#2526=AXIS2_PLACEMENT_3D('',#3727,#2985,#2986);
#2527=AXIS2_PLACEMENT_3D('',#3729,#2987,#2988);
#2528=AXIS2_PLACEMENT_3D('',#3733,#2990,#2991);
#2529=AXIS2_PLACEMENT_3D('',#3737,#2993,#2994);
#2530=AXIS2_PLACEMENT_3D('',#3739,#2995,#2996);
#2531=AXIS2_PLACEMENT_3D('',#3741,#2997,#2998);
#2532=AXIS2_PLACEMENT_3D('',#3745,#3000,#3001);
#2533=AXIS2_PLACEMENT_3D('',#3748,#3003,#3004);
#2534=AXIS2_PLACEMENT_3D('',#3749,#3005,#3006);
#2535=AXIS2_PLACEMENT_3D('',#3754,#3009,#3010);
#2536=AXIS2_PLACEMENT_3D('',#3755,#3011,#3012);
#2537=AXIS2_PLACEMENT_3D('',#3760,#3015,#3016);
#2538=AXIS2_PLACEMENT_3D('',#3761,#3017,#3018);
#2539=AXIS2_PLACEMENT_3D('',#3766,#3021,#3022);
#2540=AXIS2_PLACEMENT_3D('',#3767,#3023,#3024);
#2541=AXIS2_PLACEMENT_3D('',#3772,#3027,#3028);
#2542=AXIS2_PLACEMENT_3D('',#3773,#3029,#3030);
#2543=AXIS2_PLACEMENT_3D('',#3778,#3033,#3034);
#2544=AXIS2_PLACEMENT_3D('',#3779,#3035,#3036);
#2545=AXIS2_PLACEMENT_3D('',#3783,#3038,#3039);
#2546=AXIS2_PLACEMENT_3D('',#3785,#3041,#3042);
#2547=AXIS2_PLACEMENT_3D('',#3788,#3044,#3045);
#2548=AXIS2_PLACEMENT_3D('',#3789,#3046,#3047);
#2549=AXIS2_PLACEMENT_3D('',#3791,#3048,#3049);
#2550=AXIS2_PLACEMENT_3D('',#3793,#3051,#3052);
#2551=AXIS2_PLACEMENT_3D('',#3796,#3054,#3055);
#2552=AXIS2_PLACEMENT_3D('',#3797,#3056,#3057);
#2553=AXIS2_PLACEMENT_3D('',#3800,#3059,#3060);
#2554=AXIS2_PLACEMENT_3D('',#3801,#3061,#3062);
#2555=AXIS2_PLACEMENT_3D('',#3804,#3064,#3065);
#2556=AXIS2_PLACEMENT_3D('',#3805,#3066,#3067);
#2557=AXIS2_PLACEMENT_3D('',#3808,#3069,#3070);
#2558=AXIS2_PLACEMENT_3D('',#3809,#3071,#3072);
#2559=AXIS2_PLACEMENT_3D('',#3813,#3074,#3075);
#2560=AXIS2_PLACEMENT_3D('',#3816,#3077,#3078);
#2561=AXIS2_PLACEMENT_3D('',#3820,#3080,#3081);
#2562=AXIS2_PLACEMENT_3D('',#3823,#3083,#3084);
#2563=AXIS2_PLACEMENT_3D('',#3827,#3086,#3087);
#2564=AXIS2_PLACEMENT_3D('',#3830,#3089,#3090);
#2565=AXIS2_PLACEMENT_3D('',#3834,#3092,#3093);
#2566=AXIS2_PLACEMENT_3D('',#3837,#3095,#3096);
#2567=AXIS2_PLACEMENT_3D('',#3841,#3098,#3099);
#2568=AXIS2_PLACEMENT_3D('',#3844,#3101,#3102);
#2569=AXIS2_PLACEMENT_3D('',#3846,#3103,#3104);
#2570=AXIS2_PLACEMENT_3D('',#3850,#3106,#3107);
#2571=AXIS2_PLACEMENT_3D('',#3852,#3109,#3110);
#2572=AXIS2_PLACEMENT_3D('',#3854,#3112,#3113);
#2573=AXIS2_PLACEMENT_3D('',#3856,#3115,#3116);
#2574=AXIS2_PLACEMENT_3D('',#3858,#3118,#3119);
#2575=AXIS2_PLACEMENT_3D('',#3860,#3121,#3122);
#2576=AXIS2_PLACEMENT_3D('',#3861,#3123,#3124);
#2577=AXIS2_PLACEMENT_3D('',#3864,#3127,#3128);
#2578=AXIS2_PLACEMENT_3D('',#3866,#3130,#3131);
#2579=AXIS2_PLACEMENT_3D('',#3867,#3132,#3133);
#2580=AXIS2_PLACEMENT_3D('',#3870,#3136,#3137);
#2581=AXIS2_PLACEMENT_3D('',#3872,#3139,#3140);
#2582=AXIS2_PLACEMENT_3D('',#3873,#3141,#3142);
#2583=AXIS2_PLACEMENT_3D('',#3874,#3143,#3144);
#2584=AXIS2_PLACEMENT_3D('',#3875,#3145,#3146);
#2585=AXIS2_PLACEMENT_3D('',#3878,#3149,#3150);
#2586=AXIS2_PLACEMENT_3D('',#3880,#3152,#3153);
#2587=AXIS2_PLACEMENT_3D('',#3881,#3154,#3155);
#2588=AXIS2_PLACEMENT_3D('',#3884,#3158,#3159);
#2589=AXIS2_PLACEMENT_3D('',#3886,#3161,#3162);
#2590=AXIS2_PLACEMENT_3D('',#3887,#3163,#3164);
#2591=AXIS2_PLACEMENT_3D('',#3888,#3165,#3166);
#2592=AXIS2_PLACEMENT_3D('',#3889,#3167,#3168);
#2593=AXIS2_PLACEMENT_3D('',#3891,#3170,#3171);
#2594=AXIS2_PLACEMENT_3D('',#3893,#3173,#3174);
#2595=AXIS2_PLACEMENT_3D('',#3894,#3175,#3176);
#2596=AXIS2_PLACEMENT_3D('',#3895,#3177,#3178);
#2597=AXIS2_PLACEMENT_3D('',#3904,#3183,#3184);
#2598=AXIS2_PLACEMENT_3D('',#3906,#3185,#3186);
#2599=AXIS2_PLACEMENT_3D('',#3910,#3189,#3190);
#2600=AXIS2_PLACEMENT_3D('',#3916,#3194,#3195);
#2601=AXIS2_PLACEMENT_3D('',#3918,#3197,#3198);
#2602=AXIS2_PLACEMENT_3D('',#3919,#3199,#3200);
#2603=AXIS2_PLACEMENT_3D('',#3920,#3201,#3202);
#2604=AXIS2_PLACEMENT_3D('',#3922,#3203,#3204);
#2605=AXIS2_PLACEMENT_3D('',#3925,#3206,#3207);
#2606=AXIS2_PLACEMENT_3D('',#3926,#3208,#3209);
#2607=AXIS2_PLACEMENT_3D('',#3928,#3210,#3211);
#2608=AXIS2_PLACEMENT_3D('',#3929,#3212,#3213);
#2609=AXIS2_PLACEMENT_3D('',#3931,#3214,#3215);
#2610=AXIS2_PLACEMENT_3D('',#3932,#3216,#3217);
#2611=AXIS2_PLACEMENT_3D('',#3934,#3218,#3219);
#2612=AXIS2_PLACEMENT_3D('',#3936,#3221,#3222);
#2613=AXIS2_PLACEMENT_3D('',#3938,#3223,#3224);
#2614=AXIS2_PLACEMENT_3D('',#3940,#3225,#3226);
#2615=AXIS2_PLACEMENT_3D('',#3941,#3227,#3228);
#2616=AXIS2_PLACEMENT_3D('',#3944,#3230,#3231);
#2617=AXIS2_PLACEMENT_3D('',#3945,#3232,#3233);
#2618=AXIS2_PLACEMENT_3D('',#3946,#3234,#3235);
#2619=AXIS2_PLACEMENT_3D('',#3948,#3237,#3238);
#2620=AXIS2_PLACEMENT_3D('',#3949,#3239,#3240);
#2621=AXIS2_PLACEMENT_3D('',#3950,#3241,#3242);
#2622=AXIS2_PLACEMENT_3D('',#3959,#3247,#3248);
#2623=AXIS2_PLACEMENT_3D('',#3965,#3252,#3253);
#2624=AXIS2_PLACEMENT_3D('',#3971,#3257,#3258);
#2625=AXIS2_PLACEMENT_3D('',#3974,#3261,#3262);
#2626=AXIS2_PLACEMENT_3D('',#3975,#3263,#3264);
#2627=AXIS2_PLACEMENT_3D('',#3976,#3265,#3266);
#2628=AXIS2_PLACEMENT_3D('',#3977,#3267,#3268);
#2629=AXIS2_PLACEMENT_3D('',#3979,#3269,#3270);
#2630=AXIS2_PLACEMENT_3D('',#3981,#3271,#3272);
#2631=AXIS2_PLACEMENT_3D('',#3982,#3273,#3274);
#2632=AXIS2_PLACEMENT_3D('',#3984,#3275,#3276);
#2633=AXIS2_PLACEMENT_3D('',#3986,#3277,#3278);
#2634=AXIS2_PLACEMENT_3D('',#3987,#3279,#3280);
#2635=AXIS2_PLACEMENT_3D('',#3989,#3282,#3283);
#2636=AXIS2_PLACEMENT_3D('',#3992,#3285,#3286);
#2637=AXIS2_PLACEMENT_3D('',#3993,#3287,#3288);
#2638=AXIS2_PLACEMENT_3D('',#3995,#3289,#3290);
#2639=AXIS2_PLACEMENT_3D('',#3998,#3292,#3293);
#2640=AXIS2_PLACEMENT_3D('',#3999,#3294,#3295);
#2641=AXIS2_PLACEMENT_3D('',#4001,#3296,#3297);
#2642=AXIS2_PLACEMENT_3D('',#4002,#3298,#3299);
#2643=AXIS2_PLACEMENT_3D('',#4004,#3300,#3301);
#2644=AXIS2_PLACEMENT_3D('',#4005,#3302,#3303);
#2645=AXIS2_PLACEMENT_3D('',#4007,#3304,#3305);
#2646=AXIS2_PLACEMENT_3D('',#4009,#3307,#3308);
#2647=AXIS2_PLACEMENT_3D('',#4011,#3309,#3310);
#2648=AXIS2_PLACEMENT_3D('',#4012,#3311,#3312);
#2649=AXIS2_PLACEMENT_3D('',#4015,#3314,#3315);
#2650=AXIS2_PLACEMENT_3D('',#4016,#3316,#3317);
#2651=AXIS2_PLACEMENT_3D('',#4017,#3318,#3319);
#2652=AXIS2_PLACEMENT_3D('',#4019,#3321,#3322);
#2653=AXIS2_PLACEMENT_3D('',#4020,#3323,#3324);
#2654=AXIS2_PLACEMENT_3D('',#4021,#3325,#3326);
#2655=AXIS2_PLACEMENT_3D('',#4023,#3327,#3328);
#2656=AXIS2_PLACEMENT_3D('',#4026,#3330,#3331);
#2657=AXIS2_PLACEMENT_3D('',#4027,#3332,#3333);
#2658=AXIS2_PLACEMENT_3D('',#4029,#3334,#3335);
#2659=AXIS2_PLACEMENT_3D('',#4032,#3337,#3338);
#2660=AXIS2_PLACEMENT_3D('',#4033,#3339,#3340);
#2661=AXIS2_PLACEMENT_3D('',#4034,#3341,#3342);
#2662=AXIS2_PLACEMENT_3D('',#4035,#3343,#3344);
#2663=AXIS2_PLACEMENT_3D('',#4036,#3345,#3346);
#2664=AXIS2_PLACEMENT_3D('',#4038,#3347,#3348);
#2665=AXIS2_PLACEMENT_3D('',#4041,#3350,#3351);
#2666=AXIS2_PLACEMENT_3D('',#4042,#3352,#3353);
#2667=AXIS2_PLACEMENT_3D('',#4044,#3354,#3355);
#2668=AXIS2_PLACEMENT_3D('',#4047,#3357,#3358);
#2669=AXIS2_PLACEMENT_3D('',#4048,#3359,#3360);
#2670=AXIS2_PLACEMENT_3D('',#4049,#3361,#3362);
#2671=AXIS2_PLACEMENT_3D('',#4050,#3363,#3364);
#2672=AXIS2_PLACEMENT_3D('',#4051,#3365,#3366);
#2673=AXIS2_PLACEMENT_3D('',#4053,#3367,#3368);
#2674=AXIS2_PLACEMENT_3D('',#4056,#3370,#3371);
#2675=AXIS2_PLACEMENT_3D('',#4057,#3372,#3373);
#2676=AXIS2_PLACEMENT_3D('',#4059,#3374,#3375);
#2677=AXIS2_PLACEMENT_3D('',#4062,#3377,#3378);
#2678=AXIS2_PLACEMENT_3D('',#4063,#3379,#3380);
#2679=AXIS2_PLACEMENT_3D('',#4064,#3381,#3382);
#2680=AXIS2_PLACEMENT_3D('',#4065,#3383,#3384);
#2681=AXIS2_PLACEMENT_3D('',#4066,#3385,#3386);
#2682=AXIS2_PLACEMENT_3D('',#4068,#3387,#3388);
#2683=AXIS2_PLACEMENT_3D('',#4071,#3390,#3391);
#2684=AXIS2_PLACEMENT_3D('',#4072,#3392,#3393);
#2685=AXIS2_PLACEMENT_3D('',#4074,#3394,#3395);
#2686=AXIS2_PLACEMENT_3D('',#4077,#3397,#3398);
#2687=AXIS2_PLACEMENT_3D('',#4078,#3399,#3400);
#2688=AXIS2_PLACEMENT_3D('',#4079,#3401,#3402);
#2689=AXIS2_PLACEMENT_3D('',#4080,#3403,#3404);
#2690=AXIS2_PLACEMENT_3D('',#4081,#3405,#3406);
#2691=AXIS2_PLACEMENT_3D('',#4090,#3411,#3412);
#2692=AXIS2_PLACEMENT_3D('',#4099,#3417,#3418);
#2693=AXIS2_PLACEMENT_3D('',#4100,#3419,#3420);
#2694=AXIS2_PLACEMENT_3D('',#4101,#3421,#3422);
#2695=AXIS2_PLACEMENT_3D('',#4102,#3423,#3424);
#2696=AXIS2_PLACEMENT_3D('',#4103,#3425,#3426);
#2697=AXIS2_PLACEMENT_3D('',#4104,#3427,#3428);
#2698=AXIS2_PLACEMENT_3D('',#4105,#3429,#3430);
#2699=AXIS2_PLACEMENT_3D('',#4106,#3431,#3432);
#2700=AXIS2_PLACEMENT_3D('',#4107,#3433,#3434);
#2701=AXIS2_PLACEMENT_3D('',#4108,#3435,#3436);
#2702=AXIS2_PLACEMENT_3D('',#4109,#3437,#3438);
#2703=AXIS2_PLACEMENT_3D('',#4110,#3439,#3440);
#2704=AXIS2_PLACEMENT_3D('',#4111,#3441,#3442);
#2705=AXIS2_PLACEMENT_3D('',#4112,#3443,#3444);
#2706=AXIS2_PLACEMENT_3D('',#4113,#3445,#3446);
#2707=AXIS2_PLACEMENT_3D('',#4114,#3447,#3448);
#2708=AXIS2_PLACEMENT_3D('',#4115,#3449,#3450);
#2709=AXIS2_PLACEMENT_3D('',#4116,#3451,#3452);
#2710=AXIS2_PLACEMENT_3D('',#4117,#3453,#3454);
#2711=AXIS2_PLACEMENT_3D('',#4118,#3455,#3456);
#2712=AXIS2_PLACEMENT_3D('',#4119,#3457,#3458);
#2713=AXIS2_PLACEMENT_3D('',#4120,#3459,#3460);
#2714=AXIS2_PLACEMENT_3D('',#4121,#3461,#3462);
#2715=AXIS2_PLACEMENT_3D('',#4122,#3463,#3464);
#2716=AXIS2_PLACEMENT_3D('',#4123,#3465,#3466);
#2717=DIRECTION('axis',(0.,0.,1.));
#2718=DIRECTION('refdir',(1.,0.,0.));
#2719=DIRECTION('axis',(0.,0.,1.));
#2720=DIRECTION('refdir',(1.,0.,0.));
#2721=DIRECTION('center_axis',(0.,0.,-1.));
#2722=DIRECTION('ref_axis',(1.,0.,0.));
#2723=DIRECTION('center_axis',(0.,0.,-1.));
#2724=DIRECTION('ref_axis',(1.,0.,0.));
#2725=DIRECTION('',(0.,0.,-1.));
#2726=DIRECTION('center_axis',(0.,0.,1.));
#2727=DIRECTION('ref_axis',(1.,0.,0.));
#2728=DIRECTION('center_axis',(0.,0.,-1.));
#2729=DIRECTION('ref_axis',(1.,0.,0.));
#2730=DIRECTION('center_axis',(0.,0.,-1.));
#2731=DIRECTION('ref_axis',(1.,0.,0.));
#2732=DIRECTION('',(0.,0.,-1.));
#2733=DIRECTION('center_axis',(0.,0.,1.));
#2734=DIRECTION('ref_axis',(1.,0.,0.));
#2735=DIRECTION('center_axis',(0.,0.,-1.));
#2736=DIRECTION('ref_axis',(1.,0.,0.));
#2737=DIRECTION('center_axis',(0.,0.,-1.));
#2738=DIRECTION('ref_axis',(1.,0.,0.));
#2739=DIRECTION('',(0.,0.,-1.));
#2740=DIRECTION('center_axis',(0.,0.,1.));
#2741=DIRECTION('ref_axis',(1.,0.,0.));
#2742=DIRECTION('center_axis',(0.,0.,-1.));
#2743=DIRECTION('ref_axis',(1.,0.,0.));
#2744=DIRECTION('center_axis',(0.,0.,-1.));
#2745=DIRECTION('ref_axis',(1.,0.,0.));
#2746=DIRECTION('',(0.,0.,-1.));
#2747=DIRECTION('center_axis',(0.,0.,1.));
#2748=DIRECTION('ref_axis',(1.,0.,0.));
#2749=DIRECTION('center_axis',(0.,0.,-1.));
#2750=DIRECTION('ref_axis',(1.,0.,0.));
#2751=DIRECTION('center_axis',(0.,0.,-1.));
#2752=DIRECTION('ref_axis',(1.,0.,0.));
#2753=DIRECTION('',(0.,0.,-1.));
#2754=DIRECTION('center_axis',(0.,0.,1.));
#2755=DIRECTION('ref_axis',(1.,0.,0.));
#2756=DIRECTION('center_axis',(0.,0.,-1.));
#2757=DIRECTION('ref_axis',(1.,0.,0.));
#2758=DIRECTION('center_axis',(0.,0.,-1.));
#2759=DIRECTION('ref_axis',(1.,0.,0.));
#2760=DIRECTION('',(0.,0.,-1.));
#2761=DIRECTION('center_axis',(0.,0.,1.));
#2762=DIRECTION('ref_axis',(1.,0.,0.));
#2763=DIRECTION('center_axis',(0.,1.,0.));
#2764=DIRECTION('ref_axis',(-1.,0.,0.));
#2765=DIRECTION('',(1.,0.,0.));
#2766=DIRECTION('',(0.,0.,-1.));
#2767=DIRECTION('',(1.,0.,0.));
#2768=DIRECTION('',(0.,0.,-1.));
#2769=DIRECTION('center_axis',(1.,0.,0.));
#2770=DIRECTION('ref_axis',(0.,1.,0.));
#2771=DIRECTION('',(0.,-1.,0.));
#2772=DIRECTION('',(0.,-1.,0.));
#2773=DIRECTION('',(0.,0.,-1.));
#2774=DIRECTION('center_axis',(0.,-1.,0.));
#2775=DIRECTION('ref_axis',(1.,0.,0.));
#2776=DIRECTION('',(-1.,0.,0.));
#2777=DIRECTION('',(-1.,0.,0.));
#2778=DIRECTION('',(0.,0.,1.));
#2779=DIRECTION('center_axis',(-1.,0.,0.));
#2780=DIRECTION('ref_axis',(0.,-1.,0.));
#2781=DIRECTION('',(0.,1.,0.));
#2782=DIRECTION('',(0.,1.,0.));
#2783=DIRECTION('center_axis',(0.,0.,1.));
#2784=DIRECTION('ref_axis',(1.,0.,0.));
#2785=DIRECTION('center_axis',(0.,0.,1.));
#2786=DIRECTION('ref_axis',(1.,0.,0.));
#2787=DIRECTION('axis',(0.,0.,1.));
#2788=DIRECTION('refdir',(1.,0.,0.));
#2789=DIRECTION('center_axis',(-1.60246890531964E-16,-1.,0.));
#2790=DIRECTION('ref_axis',(1.,-1.60246890531964E-16,0.));
#2791=DIRECTION('',(-1.,1.60246890531964E-16,0.));
#2792=DIRECTION('',(0.,0.,1.));
#2793=DIRECTION('',(1.,-1.60246890531964E-16,0.));
#2794=DIRECTION('',(0.,0.,1.));
#2795=DIRECTION('center_axis',(-0.866025403784439,-0.5,0.));
#2796=DIRECTION('ref_axis',(0.5,-0.866025403784439,0.));
#2797=DIRECTION('',(-0.5,0.866025403784439,0.));
#2798=DIRECTION('',(0.5,-0.866025403784439,0.));
#2799=DIRECTION('',(0.,0.,1.));
#2800=DIRECTION('center_axis',(-0.866025403784439,0.5,0.));
#2801=DIRECTION('ref_axis',(-0.5,-0.866025403784439,0.));
#2802=DIRECTION('',(0.5,0.866025403784439,0.));
#2803=DIRECTION('',(-0.5,-0.866025403784439,0.));
#2804=DIRECTION('',(0.,0.,1.));
#2805=DIRECTION('center_axis',(1.60246890531964E-16,1.,0.));
#2806=DIRECTION('ref_axis',(-1.,1.60246890531964E-16,0.));
#2807=DIRECTION('',(1.,-1.60246890531964E-16,0.));
#2808=DIRECTION('',(-1.,1.60246890531964E-16,0.));
#2809=DIRECTION('',(0.,0.,1.));
#2810=DIRECTION('center_axis',(0.866025403784439,0.5,0.));
#2811=DIRECTION('ref_axis',(-0.5,0.866025403784439,0.));
#2812=DIRECTION('',(0.5,-0.866025403784439,0.));
#2813=DIRECTION('',(-0.5,0.866025403784439,0.));
#2814=DIRECTION('',(0.,0.,1.));
#2815=DIRECTION('center_axis',(0.866025403784439,-0.5,0.));
#2816=DIRECTION('ref_axis',(0.5,0.866025403784439,0.));
#2817=DIRECTION('',(-0.5,-0.866025403784439,0.));
#2818=DIRECTION('',(0.5,0.866025403784439,0.));
#2819=DIRECTION('center_axis',(0.,0.,1.));
#2820=DIRECTION('ref_axis',(1.,0.,0.));
#2821=DIRECTION('center_axis',(0.,0.,1.));
#2822=DIRECTION('ref_axis',(1.,0.,0.));
#2823=DIRECTION('center_axis',(0.,0.,1.));
#2824=DIRECTION('ref_axis',(1.,0.,0.));
#2825=DIRECTION('',(0.,0.,1.));
#2826=DIRECTION('center_axis',(0.,0.,1.));
#2827=DIRECTION('ref_axis',(1.,0.,0.));
#2828=DIRECTION('center_axis',(0.,0.,-1.));
#2829=DIRECTION('ref_axis',(-1.,0.,0.));
#2830=DIRECTION('center_axis',(0.,0.,-1.));
#2831=DIRECTION('ref_axis',(1.,0.,0.));
#2832=DIRECTION('center_axis',(0.,0.,1.));
#2833=DIRECTION('ref_axis',(1.,0.,0.));
#2834=DIRECTION('center_axis',(0.,0.,1.));
#2835=DIRECTION('ref_axis',(1.,0.,0.));
#2836=DIRECTION('center_axis',(0.,0.,1.));
#2837=DIRECTION('ref_axis',(1.,0.,0.));
#2838=DIRECTION('center_axis',(0.,0.,-1.));
#2839=DIRECTION('ref_axis',(1.,0.,0.));
#2840=DIRECTION('',(0.,0.,-1.));
#2841=DIRECTION('center_axis',(0.,0.,-1.));
#2842=DIRECTION('ref_axis',(1.,0.,0.));
#2843=DIRECTION('center_axis',(0.,0.,-1.));
#2844=DIRECTION('ref_axis',(1.,0.,0.));
#2845=DIRECTION('',(0.,0.,-1.));
#2846=DIRECTION('center_axis',(0.,0.,1.));
#2847=DIRECTION('ref_axis',(1.,0.,0.));
#2848=DIRECTION('center_axis',(0.,0.,1.));
#2849=DIRECTION('ref_axis',(1.,0.,0.));
#2850=DIRECTION('center_axis',(0.,0.,1.));
#2851=DIRECTION('ref_axis',(1.,0.,0.));
#2852=DIRECTION('',(0.5,-0.866025403784439,0.));
#2853=DIRECTION('',(-0.5,-0.866025403784439,0.));
#2854=DIRECTION('center_axis',(0.,0.,-1.));
#2855=DIRECTION('ref_axis',(-1.,0.,0.));
#2856=DIRECTION('center_axis',(0.,0.,1.));
#2857=DIRECTION('ref_axis',(1.,0.,0.));
#2858=DIRECTION('',(0.5,0.866025403784439,0.));
#2859=DIRECTION('',(-0.5,0.866025403784439,0.));
#2860=DIRECTION('center_axis',(-0.866025403784439,0.5,0.));
#2861=DIRECTION('ref_axis',(0.5,0.866025403784439,0.));
#2862=DIRECTION('',(0.,0.,-1.));
#2863=DIRECTION('',(0.5,0.866025403784439,0.));
#2864=DIRECTION('',(0.,0.,-1.));
#2865=DIRECTION('',(-0.5,-0.866025403784439,0.));
#2866=DIRECTION('center_axis',(-0.866025403784439,-0.5,0.));
#2867=DIRECTION('ref_axis',(-0.5,0.866025403784439,0.));
#2868=DIRECTION('',(0.,0.,1.));
#2869=DIRECTION('',(0.5,-0.866025403784439,0.));
#2870=DIRECTION('',(-0.5,0.866025403784439,0.));
#2871=DIRECTION('center_axis',(0.,0.,1.));
#2872=DIRECTION('ref_axis',(1.,0.,0.));
#2873=DIRECTION('center_axis',(0.,0.,1.));
#2874=DIRECTION('ref_axis',(1.,0.,0.));
#2875=DIRECTION('center_axis',(0.,0.,1.));
#2876=DIRECTION('ref_axis',(1.,0.,0.));
#2877=DIRECTION('center_axis',(0.,0.,1.));
#2878=DIRECTION('ref_axis',(1.,0.,0.));
#2879=DIRECTION('center_axis',(0.,0.,1.));
#2880=DIRECTION('ref_axis',(1.,0.,0.));
#2881=DIRECTION('center_axis',(0.,0.,1.));
#2882=DIRECTION('ref_axis',(1.,0.,0.));
#2883=DIRECTION('center_axis',(0.,0.,1.));
#2884=DIRECTION('ref_axis',(1.,0.,0.));
#2885=DIRECTION('center_axis',(0.,0.,1.));
#2886=DIRECTION('ref_axis',(1.,0.,0.));
#2887=DIRECTION('center_axis',(0.,0.,1.));
#2888=DIRECTION('ref_axis',(-1.,-1.22464679914735E-16,0.));
#2889=DIRECTION('center_axis',(0.,0.,1.));
#2890=DIRECTION('ref_axis',(1.,0.,0.));
#2891=DIRECTION('',(0.,0.,-1.));
#2892=DIRECTION('center_axis',(0.,0.,-1.));
#2893=DIRECTION('ref_axis',(1.,0.,0.));
#2894=DIRECTION('center_axis',(0.,0.,1.));
#2895=DIRECTION('ref_axis',(1.,0.,0.));
#2896=DIRECTION('center_axis',(0.,0.,-1.));
#2897=DIRECTION('ref_axis',(1.,0.,0.));
#2898=DIRECTION('center_axis',(0.,0.,1.));
#2899=DIRECTION('ref_axis',(1.,0.,0.));
#2900=DIRECTION('center_axis',(0.,0.,-1.));
#2901=DIRECTION('ref_axis',(1.,0.,0.));
#2902=DIRECTION('center_axis',(0.,0.,1.));
#2903=DIRECTION('ref_axis',(1.,0.,0.));
#2904=DIRECTION('',(0.,0.,-1.));
#2905=DIRECTION('center_axis',(0.,0.,1.));
#2906=DIRECTION('ref_axis',(1.,0.,0.));
#2907=DIRECTION('',(0.,0.,-1.));
#2908=DIRECTION('center_axis',(0.,0.,1.));
#2909=DIRECTION('ref_axis',(1.,0.,0.));
#2910=DIRECTION('center_axis',(0.,0.,1.));
#2911=DIRECTION('ref_axis',(1.,0.,0.));
#2912=DIRECTION('center_axis',(0.,0.,1.));
#2913=DIRECTION('ref_axis',(1.,0.,0.));
#2914=DIRECTION('',(0.,0.,-1.));
#2915=DIRECTION('center_axis',(0.,0.,1.));
#2916=DIRECTION('ref_axis',(1.,0.,0.));
#2917=DIRECTION('center_axis',(0.,0.,1.));
#2918=DIRECTION('ref_axis',(1.,0.,0.));
#2919=DIRECTION('axis',(0.,0.,1.));
#2920=DIRECTION('refdir',(1.,0.,0.));
#2921=DIRECTION('center_axis',(0.,1.,0.));
#2922=DIRECTION('ref_axis',(1.,0.,0.));
#2923=DIRECTION('',(0.,0.,1.));
#2924=DIRECTION('',(-1.,0.,0.));
#2925=DIRECTION('',(0.,0.,-1.));
#2926=DIRECTION('',(1.,0.,0.));
#2927=DIRECTION('center_axis',(0.,-1.,0.));
#2928=DIRECTION('ref_axis',(-1.,0.,0.));
#2929=DIRECTION('',(0.,0.,-1.));
#2930=DIRECTION('',(-1.,0.,0.));
#2931=DIRECTION('',(0.,0.,-1.));
#2932=DIRECTION('',(1.,0.,0.));
#2933=DIRECTION('center_axis',(1.,0.,0.));
#2934=DIRECTION('ref_axis',(0.,-1.,0.));
#2935=DIRECTION('',(0.,-1.,0.));
#2936=DIRECTION('',(0.,1.,0.));
#2937=DIRECTION('center_axis',(0.,0.,1.));
#2938=DIRECTION('ref_axis',(-1.,1.22464679914735E-16,0.));
#2939=DIRECTION('center_axis',(0.,0.,-1.));
#2940=DIRECTION('ref_axis',(1.,0.,0.));
#2941=DIRECTION('center_axis',(0.,0.,-1.));
#2942=DIRECTION('ref_axis',(1.,0.,0.));
#2943=DIRECTION('center_axis',(0.,0.,1.));
#2944=DIRECTION('ref_axis',(1.,0.,0.));
#2945=DIRECTION('center_axis',(0.,0.,-1.));
#2946=DIRECTION('ref_axis',(1.,0.,0.));
#2947=DIRECTION('center_axis',(0.,0.,1.));
#2948=DIRECTION('ref_axis',(1.,0.,0.));
#2949=DIRECTION('',(-0.5,0.866025403784439,0.));
#2950=DIRECTION('center_axis',(0.,0.,-1.));
#2951=DIRECTION('ref_axis',(0.866025403784439,0.5,0.));
#2952=DIRECTION('',(0.5,-0.866025403784439,0.));
#2953=DIRECTION('center_axis',(0.,0.,1.));
#2954=DIRECTION('ref_axis',(1.,0.,0.));
#2955=DIRECTION('center_axis',(0.,0.,-1.));
#2956=DIRECTION('ref_axis',(1.,0.,0.));
#2957=DIRECTION('center_axis',(0.,0.,1.));
#2958=DIRECTION('ref_axis',(1.,0.,0.));
#2959=DIRECTION('',(-1.,0.,0.));
#2960=DIRECTION('center_axis',(0.,0.,-1.));
#2961=DIRECTION('ref_axis',(0.,1.,0.));
#2962=DIRECTION('',(1.,0.,0.));
#2963=DIRECTION('center_axis',(0.,0.,1.));
#2964=DIRECTION('ref_axis',(1.,0.,0.));
#2965=DIRECTION('center_axis',(0.,0.,-1.));
#2966=DIRECTION('ref_axis',(1.,0.,0.));
#2967=DIRECTION('center_axis',(0.,0.,1.));
#2968=DIRECTION('ref_axis',(1.,0.,0.));
#2969=DIRECTION('',(-0.5,-0.866025403784439,0.));
#2970=DIRECTION('center_axis',(0.,0.,-1.));
#2971=DIRECTION('ref_axis',(-0.866025403784439,0.5,0.));
#2972=DIRECTION('',(0.5,0.866025403784439,0.));
#2973=DIRECTION('center_axis',(0.,0.,1.));
#2974=DIRECTION('ref_axis',(1.,0.,0.));
#2975=DIRECTION('center_axis',(0.,0.,-1.));
#2976=DIRECTION('ref_axis',(1.,0.,0.));
#2977=DIRECTION('center_axis',(0.,0.,1.));
#2978=DIRECTION('ref_axis',(1.,0.,0.));
#2979=DIRECTION('',(0.5,-0.866025403784439,0.));
#2980=DIRECTION('center_axis',(0.,0.,-1.));
#2981=DIRECTION('ref_axis',(-0.866025403784439,-0.5,0.));
#2982=DIRECTION('',(-0.5,0.866025403784439,0.));
#2983=DIRECTION('center_axis',(0.,0.,1.));
#2984=DIRECTION('ref_axis',(1.,0.,0.));
#2985=DIRECTION('center_axis',(0.,0.,-1.));
#2986=DIRECTION('ref_axis',(1.,0.,0.));
#2987=DIRECTION('center_axis',(0.,0.,1.));
#2988=DIRECTION('ref_axis',(1.,0.,0.));
#2989=DIRECTION('',(1.,-1.14850657719844E-16,0.));
#2990=DIRECTION('center_axis',(0.,0.,-1.));
#2991=DIRECTION('ref_axis',(0.,-1.,0.));
#2992=DIRECTION('',(-1.,1.14850657719844E-16,0.));
#2993=DIRECTION('center_axis',(0.,0.,1.));
#2994=DIRECTION('ref_axis',(1.,0.,0.));
#2995=DIRECTION('center_axis',(0.,0.,-1.));
#2996=DIRECTION('ref_axis',(1.,0.,0.));
#2997=DIRECTION('center_axis',(0.,0.,1.));
#2998=DIRECTION('ref_axis',(1.,0.,0.));
#2999=DIRECTION('',(0.5,0.866025403784438,0.));
#3000=DIRECTION('center_axis',(0.,0.,-1.));
#3001=DIRECTION('ref_axis',(0.866025403784438,-0.5,0.));
#3002=DIRECTION('',(-0.5,-0.866025403784439,0.));
#3003=DIRECTION('center_axis',(0.,0.,1.));
#3004=DIRECTION('ref_axis',(1.,0.,0.));
#3005=DIRECTION('center_axis',(0.,0.,-1.));
#3006=DIRECTION('ref_axis',(1.,0.,0.));
#3007=DIRECTION('',(0.,0.,-1.));
#3008=DIRECTION('',(0.,0.,1.));
#3009=DIRECTION('center_axis',(0.,0.,1.));
#3010=DIRECTION('ref_axis',(1.,0.,0.));
#3011=DIRECTION('center_axis',(0.,0.,-1.));
#3012=DIRECTION('ref_axis',(1.,0.,0.));
#3013=DIRECTION('',(0.,0.,-1.));
#3014=DIRECTION('',(0.,0.,1.));
#3015=DIRECTION('center_axis',(0.,0.,1.));
#3016=DIRECTION('ref_axis',(1.,0.,0.));
#3017=DIRECTION('center_axis',(0.,0.,-1.));
#3018=DIRECTION('ref_axis',(-0.866025403784439,-0.499999999999999,0.));
#3019=DIRECTION('',(0.,0.,-1.));
#3020=DIRECTION('',(0.,0.,1.));
#3021=DIRECTION('center_axis',(0.,0.,1.));
#3022=DIRECTION('ref_axis',(1.,0.,0.));
#3023=DIRECTION('center_axis',(0.,0.,-1.));
#3024=DIRECTION('ref_axis',(1.,0.,0.));
#3025=DIRECTION('',(0.,0.,-1.));
#3026=DIRECTION('',(0.,0.,1.));
#3027=DIRECTION('center_axis',(0.,0.,1.));
#3028=DIRECTION('ref_axis',(1.,0.,0.));
#3029=DIRECTION('center_axis',(0.,0.,-1.));
#3030=DIRECTION('ref_axis',(1.,0.,0.));
#3031=DIRECTION('',(0.,0.,-1.));
#3032=DIRECTION('',(0.,0.,1.));
#3033=DIRECTION('center_axis',(0.,0.,1.));
#3034=DIRECTION('ref_axis',(1.,0.,0.));
#3035=DIRECTION('center_axis',(0.,0.,-1.));
#3036=DIRECTION('ref_axis',(-0.866025403784439,0.5,0.));
#3037=DIRECTION('',(0.,0.,1.));
#3038=DIRECTION('center_axis',(0.,0.,1.));
#3039=DIRECTION('ref_axis',(1.,0.,0.));
#3040=DIRECTION('',(0.,0.,-1.));
#3041=DIRECTION('center_axis',(0.,0.,1.));
#3042=DIRECTION('ref_axis',(1.,0.,0.));
#3043=DIRECTION('',(0.,0.,-1.));
#3044=DIRECTION('center_axis',(0.,0.,1.));
#3045=DIRECTION('ref_axis',(1.,0.,0.));
#3046=DIRECTION('center_axis',(0.,0.,1.));
#3047=DIRECTION('ref_axis',(1.,0.,0.));
#3048=DIRECTION('center_axis',(0.,0.,1.));
#3049=DIRECTION('ref_axis',(1.,0.,0.));
#3050=DIRECTION('',(0.,0.,1.));
#3051=DIRECTION('center_axis',(0.,0.,1.));
#3052=DIRECTION('ref_axis',(1.,0.,0.));
#3053=DIRECTION('',(0.,0.,-1.));
#3054=DIRECTION('center_axis',(0.,0.,1.));
#3055=DIRECTION('ref_axis',(1.,0.,0.));
#3056=DIRECTION('center_axis',(0.,0.,1.));
#3057=DIRECTION('ref_axis',(1.,0.,0.));
#3058=DIRECTION('',(0.,0.,-1.));
#3059=DIRECTION('center_axis',(0.,0.,1.));
#3060=DIRECTION('ref_axis',(1.,0.,0.));
#3061=DIRECTION('center_axis',(0.,0.,1.));
#3062=DIRECTION('ref_axis',(1.,0.,0.));
#3063=DIRECTION('',(0.,0.,-1.));
#3064=DIRECTION('center_axis',(0.,0.,1.));
#3065=DIRECTION('ref_axis',(1.,0.,0.));
#3066=DIRECTION('center_axis',(0.,0.,1.));
#3067=DIRECTION('ref_axis',(1.,0.,0.));
#3068=DIRECTION('',(0.,0.,-1.));
#3069=DIRECTION('center_axis',(0.,0.,1.));
#3070=DIRECTION('ref_axis',(1.,0.,0.));
#3071=DIRECTION('center_axis',(0.,0.,1.));
#3072=DIRECTION('ref_axis',(1.,0.,0.));
#3073=DIRECTION('',(0.5,0.866025403784439,0.));
#3074=DIRECTION('center_axis',(0.,0.,1.));
#3075=DIRECTION('ref_axis',(0.866025403784438,-0.5,0.));
#3076=DIRECTION('',(-0.5,-0.866025403784438,0.));
#3077=DIRECTION('center_axis',(0.,0.,1.));
#3078=DIRECTION('ref_axis',(1.,0.,0.));
#3079=DIRECTION('',(1.,-1.14850657719844E-16,0.));
#3080=DIRECTION('center_axis',(0.,0.,1.));
#3081=DIRECTION('ref_axis',(0.,-1.,0.));
#3082=DIRECTION('',(-1.,1.14850657719844E-16,0.));
#3083=DIRECTION('center_axis',(0.,0.,1.));
#3084=DIRECTION('ref_axis',(1.,0.,0.));
#3085=DIRECTION('',(0.5,-0.866025403784439,0.));
#3086=DIRECTION('center_axis',(0.,0.,1.));
#3087=DIRECTION('ref_axis',(-0.866025403784439,-0.5,0.));
#3088=DIRECTION('',(-0.5,0.866025403784439,0.));
#3089=DIRECTION('center_axis',(0.,0.,1.));
#3090=DIRECTION('ref_axis',(1.,0.,0.));
#3091=DIRECTION('',(-0.5,-0.866025403784439,0.));
#3092=DIRECTION('center_axis',(0.,0.,1.));
#3093=DIRECTION('ref_axis',(-0.866025403784439,0.5,0.));
#3094=DIRECTION('',(0.5,0.866025403784439,0.));
#3095=DIRECTION('center_axis',(0.,0.,1.));
#3096=DIRECTION('ref_axis',(1.,0.,0.));
#3097=DIRECTION('',(-1.,0.,0.));
#3098=DIRECTION('center_axis',(0.,0.,1.));
#3099=DIRECTION('ref_axis',(0.,1.,0.));
#3100=DIRECTION('',(1.,0.,0.));
#3101=DIRECTION('center_axis',(0.,0.,1.));
#3102=DIRECTION('ref_axis',(1.,0.,0.));
#3103=DIRECTION('center_axis',(0.,0.,1.));
#3104=DIRECTION('ref_axis',(1.,0.,0.));
#3105=DIRECTION('',(-0.5,0.866025403784439,0.));
#3106=DIRECTION('center_axis',(0.,0.,1.));
#3107=DIRECTION('ref_axis',(0.866025403784439,0.5,0.));
#3108=DIRECTION('',(0.5,-0.866025403784439,0.));
#3109=DIRECTION('center_axis',(0.,0.,1.));
#3110=DIRECTION('ref_axis',(1.,0.,0.));
#3111=DIRECTION('',(0.,0.,1.));
#3112=DIRECTION('center_axis',(0.,0.,1.));
#3113=DIRECTION('ref_axis',(1.,0.,0.));
#3114=DIRECTION('',(0.,0.,-1.));
#3115=DIRECTION('center_axis',(-0.866025403784439,-0.5,0.));
#3116=DIRECTION('ref_axis',(-0.5,0.866025403784439,0.));
#3117=DIRECTION('',(0.,0.,-1.));
#3118=DIRECTION('center_axis',(0.866025403784439,0.5,0.));
#3119=DIRECTION('ref_axis',(0.5,-0.866025403784439,0.));
#3120=DIRECTION('',(0.,0.,-1.));
#3121=DIRECTION('center_axis',(0.,0.,-1.));
#3122=DIRECTION('ref_axis',(0.866025403784439,0.5,0.));
#3123=DIRECTION('center_axis',(-0.866025403784438,0.5,0.));
#3124=DIRECTION('ref_axis',(0.5,0.866025403784438,0.));
#3125=DIRECTION('',(0.,0.,1.));
#3126=DIRECTION('',(0.,0.,-1.));
#3127=DIRECTION('center_axis',(0.866025403784439,-0.5,0.));
#3128=DIRECTION('ref_axis',(-0.5,-0.866025403784439,0.));
#3129=DIRECTION('',(0.,0.,-1.));
#3130=DIRECTION('center_axis',(0.,0.,-1.));
#3131=DIRECTION('ref_axis',(0.866025403784438,-0.5,0.));
#3132=DIRECTION('center_axis',(1.14850657719844E-16,1.,0.));
#3133=DIRECTION('ref_axis',(1.,-1.14850657719844E-16,0.));
#3134=DIRECTION('',(0.,0.,1.));
#3135=DIRECTION('',(0.,0.,-1.));
#3136=DIRECTION('center_axis',(-1.14850657719844E-16,-1.,0.));
#3137=DIRECTION('ref_axis',(-1.,1.14850657719844E-16,0.));
#3138=DIRECTION('',(0.,0.,-1.));
#3139=DIRECTION('center_axis',(0.,0.,-1.));
#3140=DIRECTION('ref_axis',(0.,-1.,0.));
#3141=DIRECTION('center_axis',(0.,0.,1.));
#3142=DIRECTION('ref_axis',(1.,0.,0.));
#3143=DIRECTION('center_axis',(0.,0.,1.));
#3144=DIRECTION('ref_axis',(1.,0.,0.));
#3145=DIRECTION('center_axis',(0.866025403784439,0.5,0.));
#3146=DIRECTION('ref_axis',(0.5,-0.866025403784439,0.));
#3147=DIRECTION('',(0.,0.,1.));
#3148=DIRECTION('',(0.,0.,-1.));
#3149=DIRECTION('center_axis',(-0.866025403784439,-0.5,0.));
#3150=DIRECTION('ref_axis',(-0.5,0.866025403784439,0.));
#3151=DIRECTION('',(0.,0.,-1.));
#3152=DIRECTION('center_axis',(0.,0.,-1.));
#3153=DIRECTION('ref_axis',(-0.866025403784439,-0.5,0.));
#3154=DIRECTION('center_axis',(0.866025403784439,-0.5,0.));
#3155=DIRECTION('ref_axis',(-0.5,-0.866025403784439,0.));
#3156=DIRECTION('',(0.,0.,1.));
#3157=DIRECTION('',(0.,0.,-1.));
#3158=DIRECTION('center_axis',(-0.866025403784439,0.5,0.));
#3159=DIRECTION('ref_axis',(0.5,0.866025403784439,0.));
#3160=DIRECTION('',(0.,0.,-1.));
#3161=DIRECTION('center_axis',(0.,0.,-1.));
#3162=DIRECTION('ref_axis',(-0.866025403784439,0.5,0.));
#3163=DIRECTION('center_axis',(0.,0.,1.));
#3164=DIRECTION('ref_axis',(1.,0.,0.));
#3165=DIRECTION('center_axis',(0.,0.,1.));
#3166=DIRECTION('ref_axis',(1.,0.,0.));
#3167=DIRECTION('center_axis',(0.,-1.,0.));
#3168=DIRECTION('ref_axis',(-1.,0.,0.));
#3169=DIRECTION('',(0.,0.,-1.));
#3170=DIRECTION('center_axis',(0.,1.,0.));
#3171=DIRECTION('ref_axis',(1.,0.,0.));
#3172=DIRECTION('',(0.,0.,-1.));
#3173=DIRECTION('center_axis',(0.,0.,-1.));
#3174=DIRECTION('ref_axis',(0.,1.,0.));
#3175=DIRECTION('axis',(0.,0.,1.));
#3176=DIRECTION('refdir',(1.,0.,0.));
#3177=DIRECTION('center_axis',(0.,-1.,0.));
#3178=DIRECTION('ref_axis',(-1.,0.,0.));
#3179=DIRECTION('',(0.,0.,1.));
#3180=DIRECTION('',(-1.,0.,0.));
#3181=DIRECTION('',(0.,0.,-1.));
#3182=DIRECTION('',(1.,0.,0.));
#3183=DIRECTION('center_axis',(0.,0.,1.));
#3184=DIRECTION('ref_axis',(1.,0.,0.));
#3185=DIRECTION('center_axis',(0.,0.,1.));
#3186=DIRECTION('ref_axis',(1.,0.,0.));
#3187=DIRECTION('',(0.,-1.,0.));
#3188=DIRECTION('',(-1.,0.,0.));
#3189=DIRECTION('center_axis',(0.,1.,0.));
#3190=DIRECTION('ref_axis',(1.,0.,0.));
#3191=DIRECTION('',(0.,0.,-1.));
#3192=DIRECTION('',(0.,0.,-1.));
#3193=DIRECTION('',(1.,0.,0.));
#3194=DIRECTION('center_axis',(-1.,0.,0.));
#3195=DIRECTION('ref_axis',(0.,1.,0.));
#3196=DIRECTION('',(0.,1.,0.));
#3197=DIRECTION('center_axis',(0.,0.,-1.));
#3198=DIRECTION('ref_axis',(-1.,0.,0.));
#3199=DIRECTION('center_axis',(0.,0.,-1.));
#3200=DIRECTION('ref_axis',(1.,0.,0.));
#3201=DIRECTION('center_axis',(0.,0.,1.));
#3202=DIRECTION('ref_axis',(1.,0.,0.));
#3203=DIRECTION('center_axis',(0.,0.,1.));
#3204=DIRECTION('ref_axis',(1.,0.,0.));
#3205=DIRECTION('',(0.,0.,1.));
#3206=DIRECTION('center_axis',(0.,0.,1.));
#3207=DIRECTION('ref_axis',(1.,0.,0.));
#3208=DIRECTION('center_axis',(0.,0.,-1.));
#3209=DIRECTION('ref_axis',(-1.,0.,0.));
#3210=DIRECTION('center_axis',(0.,0.,-1.));
#3211=DIRECTION('ref_axis',(1.,0.,0.));
#3212=DIRECTION('center_axis',(0.,0.,1.));
#3213=DIRECTION('ref_axis',(1.,0.,0.));
#3214=DIRECTION('center_axis',(0.,0.,1.));
#3215=DIRECTION('ref_axis',(1.,0.,0.));
#3216=DIRECTION('center_axis',(0.,0.,1.));
#3217=DIRECTION('ref_axis',(1.,0.,0.));
#3218=DIRECTION('center_axis',(0.,0.,1.));
#3219=DIRECTION('ref_axis',(1.,0.,0.));
#3220=DIRECTION('',(0.,0.,-1.));
#3221=DIRECTION('center_axis',(0.,0.,1.));
#3222=DIRECTION('ref_axis',(1.,0.,0.));
#3223=DIRECTION('center_axis',(0.,0.,1.));
#3224=DIRECTION('ref_axis',(1.,0.,0.));
#3225=DIRECTION('center_axis',(0.,0.,1.));
#3226=DIRECTION('ref_axis',(1.,0.,0.));
#3227=DIRECTION('center_axis',(0.,0.,1.));
#3228=DIRECTION('ref_axis',(1.,0.,0.));
#3229=DIRECTION('',(0.,0.,-1.));
#3230=DIRECTION('center_axis',(0.,0.,1.));
#3231=DIRECTION('ref_axis',(1.,0.,0.));
#3232=DIRECTION('center_axis',(0.,0.,1.));
#3233=DIRECTION('ref_axis',(1.,0.,0.));
#3234=DIRECTION('center_axis',(0.,0.,1.));
#3235=DIRECTION('ref_axis',(1.,0.,0.));
#3236=DIRECTION('',(0.,0.,-1.));
#3237=DIRECTION('center_axis',(0.,0.,1.));
#3238=DIRECTION('ref_axis',(1.,0.,0.));
#3239=DIRECTION('axis',(0.,0.,1.));
#3240=DIRECTION('refdir',(1.,0.,0.));
#3241=DIRECTION('center_axis',(0.,1.,0.));
#3242=DIRECTION('ref_axis',(-1.,0.,0.));
#3243=DIRECTION('',(-1.,0.,0.));
#3244=DIRECTION('',(0.,0.,1.));
#3245=DIRECTION('',(-1.,0.,0.));
#3246=DIRECTION('',(0.,0.,1.));
#3247=DIRECTION('center_axis',(1.,0.,0.));
#3248=DIRECTION('ref_axis',(0.,1.,0.));
#3249=DIRECTION('',(0.,1.,0.));
#3250=DIRECTION('',(0.,1.,0.));
#3251=DIRECTION('',(0.,0.,1.));
#3252=DIRECTION('center_axis',(0.,-1.,0.));
#3253=DIRECTION('ref_axis',(1.,0.,0.));
#3254=DIRECTION('',(1.,0.,0.));
#3255=DIRECTION('',(1.,0.,0.));
#3256=DIRECTION('',(0.,0.,1.));
#3257=DIRECTION('center_axis',(-1.,0.,0.));
#3258=DIRECTION('ref_axis',(0.,-1.,0.));
#3259=DIRECTION('',(0.,-1.,0.));
#3260=DIRECTION('',(0.,-1.,0.));
#3261=DIRECTION('center_axis',(0.,0.,1.));
#3262=DIRECTION('ref_axis',(1.,0.,0.));
#3263=DIRECTION('center_axis',(0.,0.,1.));
#3264=DIRECTION('ref_axis',(1.,0.,0.));
#3265=DIRECTION('axis',(0.,0.,1.));
#3266=DIRECTION('refdir',(1.,0.,0.));
#3267=DIRECTION('center_axis',(0.,0.,1.));
#3268=DIRECTION('ref_axis',(1.,0.,0.));
#3269=DIRECTION('center_axis',(0.,0.,1.));
#3270=DIRECTION('ref_axis',(1.,0.,0.));
#3271=DIRECTION('center_axis',(0.,0.,1.));
#3272=DIRECTION('ref_axis',(1.,0.,0.));
#3273=DIRECTION('center_axis',(0.,0.,1.));
#3274=DIRECTION('ref_axis',(1.,0.,0.));
#3275=DIRECTION('center_axis',(0.,0.,1.));
#3276=DIRECTION('ref_axis',(1.,0.,0.));
#3277=DIRECTION('center_axis',(0.,0.,-1.));
#3278=DIRECTION('ref_axis',(1.,0.,0.));
#3279=DIRECTION('center_axis',(0.,0.,1.));
#3280=DIRECTION('ref_axis',(1.,0.,0.));
#3281=DIRECTION('',(0.,0.,-1.));
#3282=DIRECTION('center_axis',(0.,0.,1.));
#3283=DIRECTION('ref_axis',(1.,0.,0.));
#3284=DIRECTION('',(0.,0.,-1.));
#3285=DIRECTION('center_axis',(0.,0.,1.));
#3286=DIRECTION('ref_axis',(1.,0.,0.));
#3287=DIRECTION('center_axis',(0.,0.,1.));
#3288=DIRECTION('ref_axis',(1.,0.,0.));
#3289=DIRECTION('center_axis',(0.,0.,1.));
#3290=DIRECTION('ref_axis',(1.,0.,0.));
#3291=DIRECTION('',(0.,0.,1.));
#3292=DIRECTION('center_axis',(0.,0.,1.));
#3293=DIRECTION('ref_axis',(1.,0.,0.));
#3294=DIRECTION('center_axis',(0.,0.,-1.));
#3295=DIRECTION('ref_axis',(-1.,0.,0.));
#3296=DIRECTION('center_axis',(0.,0.,-1.));
#3297=DIRECTION('ref_axis',(1.,0.,0.));
#3298=DIRECTION('center_axis',(0.,0.,1.));
#3299=DIRECTION('ref_axis',(1.,0.,0.));
#3300=DIRECTION('center_axis',(0.,0.,1.));
#3301=DIRECTION('ref_axis',(1.,0.,0.));
#3302=DIRECTION('center_axis',(0.,0.,1.));
#3303=DIRECTION('ref_axis',(1.,0.,0.));
#3304=DIRECTION('center_axis',(0.,0.,1.));
#3305=DIRECTION('ref_axis',(1.,0.,0.));
#3306=DIRECTION('',(0.,0.,-1.));
#3307=DIRECTION('center_axis',(0.,0.,1.));
#3308=DIRECTION('ref_axis',(1.,0.,0.));
#3309=DIRECTION('center_axis',(0.,0.,1.));
#3310=DIRECTION('ref_axis',(1.,0.,0.));
#3311=DIRECTION('center_axis',(0.,0.,1.));
#3312=DIRECTION('ref_axis',(1.,0.,0.));
#3313=DIRECTION('',(0.,0.,-1.));
#3314=DIRECTION('center_axis',(0.,0.,1.));
#3315=DIRECTION('ref_axis',(1.,0.,0.));
#3316=DIRECTION('center_axis',(0.,0.,1.));
#3317=DIRECTION('ref_axis',(1.,0.,0.));
#3318=DIRECTION('center_axis',(0.,0.,1.));
#3319=DIRECTION('ref_axis',(1.,0.,0.));
#3320=DIRECTION('',(0.,0.,-1.));
#3321=DIRECTION('center_axis',(0.,0.,1.));
#3322=DIRECTION('ref_axis',(1.,0.,0.));
#3323=DIRECTION('axis',(0.,0.,1.));
#3324=DIRECTION('refdir',(1.,0.,0.));
#3325=DIRECTION('center_axis',(0.,0.,1.));
#3326=DIRECTION('ref_axis',(1.,0.,0.));
#3327=DIRECTION('center_axis',(0.,0.,-1.));
#3328=DIRECTION('ref_axis',(1.,0.,0.));
#3329=DIRECTION('',(0.,0.,-1.));
#3330=DIRECTION('center_axis',(0.,0.,-1.));
#3331=DIRECTION('ref_axis',(1.,0.,0.));
#3332=DIRECTION('center_axis',(0.,0.,1.));
#3333=DIRECTION('ref_axis',(1.,0.,0.));
#3334=DIRECTION('center_axis',(0.,0.,1.));
#3335=DIRECTION('ref_axis',(1.,0.,0.));
#3336=DIRECTION('',(0.,0.,-1.));
#3337=DIRECTION('center_axis',(0.,0.,1.));
#3338=DIRECTION('ref_axis',(1.,0.,0.));
#3339=DIRECTION('center_axis',(0.,0.,1.));
#3340=DIRECTION('ref_axis',(1.,0.,0.));
#3341=DIRECTION('center_axis',(0.,0.,1.));
#3342=DIRECTION('ref_axis',(1.,0.,0.));
#3343=DIRECTION('axis',(0.,0.,1.));
#3344=DIRECTION('refdir',(1.,0.,0.));
#3345=DIRECTION('center_axis',(0.,0.,1.));
#3346=DIRECTION('ref_axis',(1.,0.,0.));
#3347=DIRECTION('center_axis',(0.,0.,-1.));
#3348=DIRECTION('ref_axis',(1.,0.,0.));
#3349=DIRECTION('',(0.,0.,-1.));
#3350=DIRECTION('center_axis',(0.,0.,-1.));
#3351=DIRECTION('ref_axis',(1.,0.,0.));
#3352=DIRECTION('center_axis',(0.,0.,1.));
#3353=DIRECTION('ref_axis',(1.,0.,0.));
#3354=DIRECTION('center_axis',(0.,0.,1.));
#3355=DIRECTION('ref_axis',(1.,0.,0.));
#3356=DIRECTION('',(0.,0.,-1.));
#3357=DIRECTION('center_axis',(0.,0.,1.));
#3358=DIRECTION('ref_axis',(1.,0.,0.));
#3359=DIRECTION('center_axis',(0.,0.,1.));
#3360=DIRECTION('ref_axis',(1.,0.,0.));
#3361=DIRECTION('center_axis',(0.,0.,1.));
#3362=DIRECTION('ref_axis',(1.,0.,0.));
#3363=DIRECTION('axis',(0.,0.,1.));
#3364=DIRECTION('refdir',(1.,0.,0.));
#3365=DIRECTION('center_axis',(0.,0.,1.));
#3366=DIRECTION('ref_axis',(1.,0.,0.));
#3367=DIRECTION('center_axis',(0.,0.,-1.));
#3368=DIRECTION('ref_axis',(1.,0.,0.));
#3369=DIRECTION('',(0.,0.,-1.));
#3370=DIRECTION('center_axis',(0.,0.,-1.));
#3371=DIRECTION('ref_axis',(1.,0.,0.));
#3372=DIRECTION('center_axis',(0.,0.,1.));
#3373=DIRECTION('ref_axis',(1.,0.,0.));
#3374=DIRECTION('center_axis',(0.,0.,1.));
#3375=DIRECTION('ref_axis',(1.,0.,0.));
#3376=DIRECTION('',(0.,0.,-1.));
#3377=DIRECTION('center_axis',(0.,0.,1.));
#3378=DIRECTION('ref_axis',(1.,0.,0.));
#3379=DIRECTION('center_axis',(0.,0.,1.));
#3380=DIRECTION('ref_axis',(1.,0.,0.));
#3381=DIRECTION('center_axis',(0.,0.,1.));
#3382=DIRECTION('ref_axis',(1.,0.,0.));
#3383=DIRECTION('axis',(0.,0.,1.));
#3384=DIRECTION('refdir',(1.,0.,0.));
#3385=DIRECTION('center_axis',(0.,0.,1.));
#3386=DIRECTION('ref_axis',(1.,0.,0.));
#3387=DIRECTION('center_axis',(0.,0.,-1.));
#3388=DIRECTION('ref_axis',(1.,0.,0.));
#3389=DIRECTION('',(0.,0.,-1.));
#3390=DIRECTION('center_axis',(0.,0.,-1.));
#3391=DIRECTION('ref_axis',(1.,0.,0.));
#3392=DIRECTION('center_axis',(0.,0.,1.));
#3393=DIRECTION('ref_axis',(1.,0.,0.));
#3394=DIRECTION('center_axis',(0.,0.,1.));
#3395=DIRECTION('ref_axis',(1.,0.,0.));
#3396=DIRECTION('',(0.,0.,-1.));
#3397=DIRECTION('center_axis',(0.,0.,1.));
#3398=DIRECTION('ref_axis',(1.,0.,0.));
#3399=DIRECTION('center_axis',(0.,0.,1.));
#3400=DIRECTION('ref_axis',(1.,0.,0.));
#3401=DIRECTION('center_axis',(0.,0.,1.));
#3402=DIRECTION('ref_axis',(1.,0.,0.));
#3403=DIRECTION('axis',(0.,0.,1.));
#3404=DIRECTION('refdir',(1.,0.,0.));
#3405=DIRECTION('center_axis',(-1.,0.,0.));
#3406=DIRECTION('ref_axis',(0.,1.,0.));
#3407=DIRECTION('',(0.,0.,1.));
#3408=DIRECTION('',(0.,-1.,0.));
#3409=DIRECTION('',(0.,0.,-1.));
#3410=DIRECTION('',(0.,1.,0.));
#3411=DIRECTION('center_axis',(1.,0.,0.));
#3412=DIRECTION('ref_axis',(0.,-1.,0.));
#3413=DIRECTION('',(0.,0.,-1.));
#3414=DIRECTION('',(0.,-1.,0.));
#3415=DIRECTION('',(0.,0.,1.));
#3416=DIRECTION('',(0.,1.,0.));
#3417=DIRECTION('center_axis',(0.,0.,1.));
#3418=DIRECTION('ref_axis',(1.,0.,0.));
#3419=DIRECTION('center_axis',(0.,0.,1.));
#3420=DIRECTION('ref_axis',(1.,0.,0.));
#3421=DIRECTION('center_axis',(0.,0.,-1.));
#3422=DIRECTION('ref_axis',(1.,0.,0.));
#3423=DIRECTION('center_axis',(0.,0.,1.));
#3424=DIRECTION('ref_axis',(6.12323399573677E-17,-1.,0.));
#3425=DIRECTION('center_axis',(0.,0.,-1.));
#3426=DIRECTION('ref_axis',(1.,0.,0.));
#3427=DIRECTION('center_axis',(0.,0.,1.));
#3428=DIRECTION('ref_axis',(6.12323399573677E-17,-1.,0.));
#3429=DIRECTION('center_axis',(0.,0.,1.));
#3430=DIRECTION('ref_axis',(1.,0.,0.));
#3431=DIRECTION('center_axis',(0.,0.,1.));
#3432=DIRECTION('ref_axis',(1.,0.,0.));
#3433=DIRECTION('',(0.,0.,1.));
#3434=DIRECTION('',(1.,0.,0.));
#3435=DIRECTION('',(0.,0.,1.));
#3436=DIRECTION('',(1.,0.,0.));
#3437=DIRECTION('',(0.,0.,1.));
#3438=DIRECTION('',(1.,0.,0.));
#3439=DIRECTION('',(0.,0.,1.));
#3440=DIRECTION('',(1.,0.,0.));
#3441=DIRECTION('',(0.,0.,1.));
#3442=DIRECTION('',(1.,0.,0.));
#3443=DIRECTION('',(0.,0.,1.));
#3444=DIRECTION('',(1.,0.,0.));
#3445=DIRECTION('',(0.,0.,1.));
#3446=DIRECTION('',(1.,0.,0.));
#3447=DIRECTION('',(0.,0.,1.));
#3448=DIRECTION('',(1.,0.,0.));
#3449=DIRECTION('',(0.,0.,1.));
#3450=DIRECTION('',(1.,0.,0.));
#3451=DIRECTION('',(0.,0.,1.));
#3452=DIRECTION('',(1.,0.,0.));
#3453=DIRECTION('',(0.,0.,1.));
#3454=DIRECTION('',(1.,0.,0.));
#3455=DIRECTION('',(0.,0.,1.));
#3456=DIRECTION('',(1.,0.,0.));
#3457=DIRECTION('',(0.,0.,1.));
#3458=DIRECTION('',(1.,0.,0.));
#3459=DIRECTION('',(0.,0.,1.));
#3460=DIRECTION('',(1.,0.,0.));
#3461=DIRECTION('',(0.,0.,1.));
#3462=DIRECTION('',(1.,0.,0.));
#3463=DIRECTION('',(0.,0.,1.));
#3464=DIRECTION('',(1.,0.,0.));
#3465=DIRECTION('',(0.,0.,1.));
#3466=DIRECTION('',(1.,0.,0.));
#3467=CARTESIAN_POINT('',(0.,0.,0.));
#3468=CARTESIAN_POINT('',(0.,0.,0.));
#3469=CARTESIAN_POINT('Origin',(180.,-90.,5.));
#3470=CARTESIAN_POINT('',(175.5,-90.,10.));
#3471=CARTESIAN_POINT('Origin',(180.,-90.,10.));
#3472=CARTESIAN_POINT('',(175.5,-90.,0.));
#3473=CARTESIAN_POINT('',(175.5,-90.,5.));
#3474=CARTESIAN_POINT('Origin',(180.,-90.,0.));
#3475=CARTESIAN_POINT('Origin',(-80.,-90.,5.));
#3476=CARTESIAN_POINT('',(-84.5,-90.,10.));
#3477=CARTESIAN_POINT('Origin',(-80.,-90.,10.));
#3478=CARTESIAN_POINT('',(-84.5,-90.,0.));
#3479=CARTESIAN_POINT('',(-84.5,-90.,5.));
#3480=CARTESIAN_POINT('Origin',(-80.,-90.,0.));
#3481=CARTESIAN_POINT('Origin',(-80.,90.,5.));
#3482=CARTESIAN_POINT('',(-84.5,90.,10.));
#3483=CARTESIAN_POINT('Origin',(-80.,90.,10.));
#3484=CARTESIAN_POINT('',(-84.5,90.,0.));
#3485=CARTESIAN_POINT('',(-84.5,90.,5.));
#3486=CARTESIAN_POINT('Origin',(-80.,90.,0.));
#3487=CARTESIAN_POINT('Origin',(180.,90.,5.));
#3488=CARTESIAN_POINT('',(175.5,90.,10.));
#3489=CARTESIAN_POINT('Origin',(180.,90.,10.));
#3490=CARTESIAN_POINT('',(175.5,90.,0.));
#3491=CARTESIAN_POINT('',(175.5,90.,5.));
#3492=CARTESIAN_POINT('Origin',(180.,90.,0.));
#3493=CARTESIAN_POINT('Origin',(0.,0.,5.));
#3494=CARTESIAN_POINT('',(-7.,8.57252759403147E-16,10.));
#3495=CARTESIAN_POINT('Origin',(0.,0.,10.));
#3496=CARTESIAN_POINT('',(-7.,8.57252759403147E-16,0.));
#3497=CARTESIAN_POINT('',(-7.,8.57252759403147E-16,5.));
#3498=CARTESIAN_POINT('Origin',(0.,0.,0.));
#3499=CARTESIAN_POINT('Origin',(100.,0.,5.));
#3500=CARTESIAN_POINT('',(93.,8.57252759403147E-16,10.));
#3501=CARTESIAN_POINT('Origin',(100.,0.,10.));
#3502=CARTESIAN_POINT('',(93.,8.57252759403147E-16,0.));
#3503=CARTESIAN_POINT('',(93.,8.57252759403147E-16,5.));
#3504=CARTESIAN_POINT('Origin',(100.,0.,0.));
#3505=CARTESIAN_POINT('Origin',(200.,115.,0.));
#3506=CARTESIAN_POINT('',(205.,115.,0.));
#3507=CARTESIAN_POINT('',(-105.,115.,0.));
#3508=CARTESIAN_POINT('',(125.,115.,0.));
#3509=CARTESIAN_POINT('',(-105.,115.,10.));
#3510=CARTESIAN_POINT('',(-105.,115.,0.));
#3511=CARTESIAN_POINT('',(205.,115.,10.));
#3512=CARTESIAN_POINT('',(125.,115.,10.));
#3513=CARTESIAN_POINT('',(205.,115.,0.));
#3514=CARTESIAN_POINT('Origin',(205.,-110.,0.));
#3515=CARTESIAN_POINT('',(205.,-115.,0.));
#3516=CARTESIAN_POINT('',(205.,-55.,0.));
#3517=CARTESIAN_POINT('',(205.,-115.,10.));
#3518=CARTESIAN_POINT('',(205.,-55.,10.));
#3519=CARTESIAN_POINT('',(205.,-115.,0.));
#3520=CARTESIAN_POINT('Origin',(-100.,-115.,0.));
#3521=CARTESIAN_POINT('',(-105.,-115.,0.));
#3522=CARTESIAN_POINT('',(-25.,-115.,0.));
#3523=CARTESIAN_POINT('',(-105.,-115.,10.));
#3524=CARTESIAN_POINT('',(-25.,-115.,10.));
#3525=CARTESIAN_POINT('',(-105.,-115.,0.));
#3526=CARTESIAN_POINT('Origin',(-105.,110.,0.));
#3527=CARTESIAN_POINT('',(-105.,55.,0.));
#3528=CARTESIAN_POINT('',(-105.,55.,10.));
#3529=CARTESIAN_POINT('Origin',(50.,0.,10.));
#3530=CARTESIAN_POINT('Origin',(50.,0.,0.));
#3531=CARTESIAN_POINT('',(0.,0.,0.));
#3532=CARTESIAN_POINT('Origin',(-1.73205080756888,-3.,60.));
#3533=CARTESIAN_POINT('',(1.73205080756888,-3.,60.));
#3534=CARTESIAN_POINT('',(-1.73205080756888,-3.,60.));
#3535=CARTESIAN_POINT('',(-0.86602540378444,-3.,60.));
#3536=CARTESIAN_POINT('',(1.73205080756888,-3.,68.));
#3537=CARTESIAN_POINT('',(1.73205080756888,-3.,60.));
#3538=CARTESIAN_POINT('',(-1.73205080756888,-3.,68.));
#3539=CARTESIAN_POINT('',(-1.73205080756888,-3.,68.));
#3540=CARTESIAN_POINT('',(-1.73205080756888,-3.,60.));
#3541=CARTESIAN_POINT('Origin',(-3.46410161513775,4.24230095489963E-16,
60.));
#3542=CARTESIAN_POINT('',(-3.46410161513775,4.24230095489963E-16,60.));
#3543=CARTESIAN_POINT('',(-3.03108891324554,-0.749999999999999,60.));
#3544=CARTESIAN_POINT('',(-3.46410161513775,5.55111512312578E-16,68.));
#3545=CARTESIAN_POINT('',(-3.46410161513775,4.24230095489963E-16,68.));
#3546=CARTESIAN_POINT('',(-3.46410161513775,4.24230095489963E-16,60.));
#3547=CARTESIAN_POINT('Origin',(-1.73205080756888,3.,60.));
#3548=CARTESIAN_POINT('',(-1.73205080756888,3.,60.));
#3549=CARTESIAN_POINT('',(-2.1650635094611,2.25,60.));
#3550=CARTESIAN_POINT('',(-1.73205080756888,3.,68.));
#3551=CARTESIAN_POINT('',(-1.73205080756888,3.,68.));
#3552=CARTESIAN_POINT('',(-1.73205080756888,3.,60.));
#3553=CARTESIAN_POINT('Origin',(1.73205080756888,3.,60.));
#3554=CARTESIAN_POINT('',(1.73205080756888,3.,60.));
#3555=CARTESIAN_POINT('',(0.866025403784439,3.,60.));
#3556=CARTESIAN_POINT('',(1.73205080756888,3.,68.));
#3557=CARTESIAN_POINT('',(1.73205080756888,3.,68.));
#3558=CARTESIAN_POINT('',(1.73205080756888,3.,60.));
#3559=CARTESIAN_POINT('Origin',(3.46410161513775,0.,60.));
#3560=CARTESIAN_POINT('',(3.46410161513775,0.,60.));
#3561=CARTESIAN_POINT('',(3.03108891324554,0.75,60.));
#3562=CARTESIAN_POINT('',(3.46410161513775,0.,68.));
#3563=CARTESIAN_POINT('',(3.46410161513775,0.,68.));
#3564=CARTESIAN_POINT('',(3.46410161513775,0.,60.));
#3565=CARTESIAN_POINT('Origin',(1.73205080756888,-3.,60.));
#3566=CARTESIAN_POINT('',(2.1650635094611,-2.25,60.));
#3567=CARTESIAN_POINT('',(1.73205080756888,-3.,68.));
#3568=CARTESIAN_POINT('Origin',(0.,5.55111512312578E-16,68.));
#3569=CARTESIAN_POINT('Origin',(0.,0.,-3.));
#3570=CARTESIAN_POINT('',(-4.,-4.89858719658941E-16,-4.));
#3571=CARTESIAN_POINT('Origin',(0.,0.,-4.));
#3572=CARTESIAN_POINT('',(-4.,-4.89858719658941E-16,-2.));
#3573=CARTESIAN_POINT('',(-4.,-4.89858719658941E-16,-3.));
#3574=CARTESIAN_POINT('Origin',(0.,0.,-2.));
#3575=CARTESIAN_POINT('Origin',(8.,0.,-4.));
#3576=CARTESIAN_POINT('',(-5.,6.12323399573677E-16,-4.));
#3577=CARTESIAN_POINT('Origin',(0.,0.,-4.));
#3578=CARTESIAN_POINT('Origin',(4.,0.,-2.));
#3579=CARTESIAN_POINT('',(-5.,-6.12323399573677E-16,-2.));
#3580=CARTESIAN_POINT('Origin',(0.,0.,-2.));
#3581=CARTESIAN_POINT('Origin',(0.,0.,-5.));
#3582=CARTESIAN_POINT('',(-5.,6.12323399573677E-16,12.));
#3583=CARTESIAN_POINT('Origin',(0.,0.,12.));
#3584=CARTESIAN_POINT('',(-5.,-6.12323399573677E-16,-5.));
#3585=CARTESIAN_POINT('Origin',(50.,0.,16.));
#3586=CARTESIAN_POINT('',(45.,6.12323399573677E-16,20.));
#3587=CARTESIAN_POINT('Origin',(50.,0.,20.));
#3588=CARTESIAN_POINT('',(45.,6.12323399573677E-16,12.));
#3589=CARTESIAN_POINT('',(45.,6.12323399573677E-16,16.));
#3590=CARTESIAN_POINT('Origin',(50.,0.,12.));
#3591=CARTESIAN_POINT('Origin',(50.,0.,44.));
#3592=CARTESIAN_POINT('',(2.49999999999999,-4.33012701892218,44.));
#3593=CARTESIAN_POINT('',(2.5,4.33012701892219,44.));
#3594=CARTESIAN_POINT('Origin',(0.,0.,44.));
#3595=CARTESIAN_POINT('',(0.,0.,44.));
#3596=CARTESIAN_POINT('',(0.,0.,44.));
#3597=CARTESIAN_POINT('',(100.,173.205080756888,44.));
#3598=CARTESIAN_POINT('Origin',(50.,0.,32.));
#3599=CARTESIAN_POINT('',(5.99999999999999,-10.3923048454132,32.));
#3600=CARTESIAN_POINT('',(6.,10.3923048454133,32.));
#3601=CARTESIAN_POINT('Origin',(0.,0.,32.));
#3602=CARTESIAN_POINT('',(0.,0.,32.));
#3603=CARTESIAN_POINT('',(100.,173.205080756888,32.));
#3604=CARTESIAN_POINT('',(0.,0.,32.));
#3605=CARTESIAN_POINT('Origin',(0.,0.,44.));
#3606=CARTESIAN_POINT('',(20.,34.6410161513775,44.));
#3607=CARTESIAN_POINT('',(20.,34.6410161513775,32.));
#3608=CARTESIAN_POINT('',(20.,34.6410161513775,32.));
#3609=CARTESIAN_POINT('',(0.,0.,44.));
#3610=CARTESIAN_POINT('',(0.,0.,44.));
#3611=CARTESIAN_POINT('',(0.,0.,32.));
#3612=CARTESIAN_POINT('Origin',(100.,-173.205080756888,44.));
#3613=CARTESIAN_POINT('',(20.,-34.6410161513775,32.));
#3614=CARTESIAN_POINT('',(20.,-34.6410161513775,44.));
#3615=CARTESIAN_POINT('',(20.,-34.6410161513775,32.));
#3616=CARTESIAN_POINT('',(50.,-86.6025403784438,32.));
#3617=CARTESIAN_POINT('',(50.,-86.6025403784438,44.));
#3618=CARTESIAN_POINT('Origin',(0.,0.,44.));
#3619=CARTESIAN_POINT('',(-5.,-6.12323399573677E-16,44.));
#3620=CARTESIAN_POINT('Origin',(0.,0.,44.));
#3621=CARTESIAN_POINT('Origin',(0.,0.,44.));
#3622=CARTESIAN_POINT('Origin',(0.,0.,44.));
#3623=CARTESIAN_POINT('Origin',(0.,0.,32.));
#3624=CARTESIAN_POINT('Origin',(0.,0.,32.));
#3625=CARTESIAN_POINT('',(-12.,-1.46957615897682E-15,32.));
#3626=CARTESIAN_POINT('Origin',(0.,0.,32.));
#3627=CARTESIAN_POINT('Origin',(0.,0.,32.));
#3628=CARTESIAN_POINT('Origin',(0.,0.,32.));
#3629=CARTESIAN_POINT('Origin',(0.,0.,20.));
#3630=CARTESIAN_POINT('',(-12.,-1.46957615897682E-15,20.));
#3631=CARTESIAN_POINT('',(-12.,-1.46957615897682E-15,20.));
#3632=CARTESIAN_POINT('Origin',(0.,0.,20.));
#3633=CARTESIAN_POINT('Origin',(0.,0.,20.));
#3634=CARTESIAN_POINT('',(-65.,7.9602041944578E-15,20.));
#3635=CARTESIAN_POINT('Origin',(0.,0.,20.));
#3636=CARTESIAN_POINT('Origin',(0.,0.,12.));
#3637=CARTESIAN_POINT('',(-65.,7.9602041944578E-15,12.));
#3638=CARTESIAN_POINT('Origin',(0.,0.,12.));
#3639=CARTESIAN_POINT('Origin',(0.,0.,12.));
#3640=CARTESIAN_POINT('',(-65.,-7.9602041944578E-15,12.));
#3641=CARTESIAN_POINT('Origin',(0.,0.,-5.));
#3642=CARTESIAN_POINT('',(-5.,-6.12323399573677E-16,-5.));
#3643=CARTESIAN_POINT('',(-5.,-6.12323399573677E-16,-5.));
#3644=CARTESIAN_POINT('Origin',(0.,0.,-5.));
#3645=CARTESIAN_POINT('Origin',(0.,0.,-5.));
#3646=CARTESIAN_POINT('',(-5.,-6.12323399573677E-16,60.));
#3647=CARTESIAN_POINT('Origin',(0.,0.,60.));
#3648=CARTESIAN_POINT('',(-5.,-6.12323399573677E-16,-5.));
#3649=CARTESIAN_POINT('Origin',(0.,0.,60.));
#3650=CARTESIAN_POINT('Origin',(0.,0.,-5.));
#3651=CARTESIAN_POINT('',(0.,0.,0.));
#3652=CARTESIAN_POINT('Origin',(3.,1.5,12.));
#3653=CARTESIAN_POINT('',(4.76969600708473,1.5,0.));
#3654=CARTESIAN_POINT('',(4.76969600708473,1.5,12.));
#3655=CARTESIAN_POINT('',(4.76969600708473,1.5,0.));
#3656=CARTESIAN_POINT('',(6.,1.5,0.));
#3657=CARTESIAN_POINT('',(1.5,1.5,0.));
#3658=CARTESIAN_POINT('',(6.,1.5,12.));
#3659=CARTESIAN_POINT('',(6.,1.5,12.));
#3660=CARTESIAN_POINT('',(1.5,1.5,12.));
#3661=CARTESIAN_POINT('Origin',(6.,-1.5,12.));
#3662=CARTESIAN_POINT('',(4.76969600708473,-1.5,12.));
#3663=CARTESIAN_POINT('',(4.76969600708473,-1.5,0.));
#3664=CARTESIAN_POINT('',(4.76969600708473,-1.5,0.));
#3665=CARTESIAN_POINT('',(6.,-1.5,12.));
#3666=CARTESIAN_POINT('',(3.,-1.5,12.));
#3667=CARTESIAN_POINT('',(6.,-1.5,0.));
#3668=CARTESIAN_POINT('',(6.,-1.5,12.));
#3669=CARTESIAN_POINT('',(3.,-1.5,0.));
#3670=CARTESIAN_POINT('Origin',(6.,1.5,12.));
#3671=CARTESIAN_POINT('',(6.,0.75,12.));
#3672=CARTESIAN_POINT('',(6.,0.75,0.));
#3673=CARTESIAN_POINT('Origin',(0.,0.,0.));
#3674=CARTESIAN_POINT('Origin',(0.,0.,12.));
#3675=CARTESIAN_POINT('Origin',(0.,0.,0.));
#3676=CARTESIAN_POINT('Origin',(0.,0.,12.));
#3677=CARTESIAN_POINT('',(-36.8837494704647,-82.095,12.));
#3678=CARTESIAN_POINT('',(36.8837494704646,-82.095,12.));
#3679=CARTESIAN_POINT('Origin',(-1.83697019872103E-14,-100.,12.));
#3680=CARTESIAN_POINT('',(39.7037362185807,-80.7688883808943,12.));
#3681=CARTESIAN_POINT('Origin',(0.,0.,12.));
#3682=CARTESIAN_POINT('',(15.8038475772934,-39.3730669589464,12.));
#3683=CARTESIAN_POINT('',(19.8038475772934,-46.3012701892219,12.));
#3684=CARTESIAN_POINT('',(26.1961524227066,-33.3730669589464,12.));
#3685=CARTESIAN_POINT('Origin',(21.,-36.3730669589464,12.));
#3686=CARTESIAN_POINT('',(50.0960410639939,-74.7688883808943,12.));
#3687=CARTESIAN_POINT('',(15.6961524227066,-15.1865334794732,12.));
#3688=CARTESIAN_POINT('',(52.6544807884511,-72.9897640282432,12.));
#3689=CARTESIAN_POINT('Origin',(0.,0.,12.));
#3690=CARTESIAN_POINT('',(89.5382302589158,-9.10523597175683,12.));
#3691=CARTESIAN_POINT('Origin',(86.6025403784438,-50.,12.));
#3692=CARTESIAN_POINT('',(89.7997772825746,-6.,12.));
#3693=CARTESIAN_POINT('Origin',(0.,0.,12.));
#3694=CARTESIAN_POINT('',(42.,-6.,12.));
#3695=CARTESIAN_POINT('',(50.,-6.,12.));
#3696=CARTESIAN_POINT('',(42.,6.,12.));
#3697=CARTESIAN_POINT('Origin',(42.,0.,12.));
#3698=CARTESIAN_POINT('',(89.7997772825746,6.,12.));
#3699=CARTESIAN_POINT('',(21.,6.,12.));
#3700=CARTESIAN_POINT('',(89.5382302589158,9.10523597175679,12.));
#3701=CARTESIAN_POINT('Origin',(0.,0.,12.));
#3702=CARTESIAN_POINT('',(52.6544807884512,72.9897640282432,12.));
#3703=CARTESIAN_POINT('Origin',(86.6025403784439,50.,12.));
#3704=CARTESIAN_POINT('',(50.0960410639939,74.7688883808943,12.));
#3705=CARTESIAN_POINT('Origin',(0.,0.,12.));
#3706=CARTESIAN_POINT('',(26.1961524227066,33.3730669589464,12.));
#3707=CARTESIAN_POINT('',(30.1961524227066,40.3012701892219,12.));
#3708=CARTESIAN_POINT('',(15.8038475772934,39.3730669589464,12.));
#3709=CARTESIAN_POINT('Origin',(21.,36.3730669589464,12.));
#3710=CARTESIAN_POINT('',(39.7037362185807,80.7688883808943,12.));
#3711=CARTESIAN_POINT('',(5.30384757729338,21.1865334794732,12.));
#3712=CARTESIAN_POINT('',(36.8837494704646,82.095,12.));
#3713=CARTESIAN_POINT('Origin',(0.,0.,12.));
#3714=CARTESIAN_POINT('',(-36.8837494704646,82.095,12.));
#3715=CARTESIAN_POINT('Origin',(6.12323399573677E-15,100.,12.));
#3716=CARTESIAN_POINT('',(-39.7037362185806,80.7688883808943,12.));
#3717=CARTESIAN_POINT('Origin',(0.,0.,12.));
#3718=CARTESIAN_POINT('',(-15.8038475772934,39.3730669589464,12.));
#3719=CARTESIAN_POINT('',(-19.8038475772934,46.3012701892219,12.));
#3720=CARTESIAN_POINT('',(-26.1961524227066,33.3730669589464,12.));
#3721=CARTESIAN_POINT('Origin',(-21.,36.3730669589464,12.));
#3722=CARTESIAN_POINT('',(-50.0960410639939,74.7688883808943,12.));
#3723=CARTESIAN_POINT('',(-15.6961524227066,15.1865334794732,12.));
#3724=CARTESIAN_POINT('',(-52.6544807884512,72.9897640282432,12.));
#3725=CARTESIAN_POINT('Origin',(0.,0.,12.));
#3726=CARTESIAN_POINT('',(-89.5382302589158,9.10523597175679,12.));
#3727=CARTESIAN_POINT('Origin',(-86.6025403784439,50.,12.));
#3728=CARTESIAN_POINT('',(-89.7997772825746,6.00000000000001,12.));
#3729=CARTESIAN_POINT('Origin',(0.,0.,12.));
#3730=CARTESIAN_POINT('',(-42.,6.00000000000001,12.));
#3731=CARTESIAN_POINT('',(-50.,6.00000000000001,12.));
#3732=CARTESIAN_POINT('',(-42.,-5.99999999999999,12.));
#3733=CARTESIAN_POINT('Origin',(-42.,5.14351655641888E-15,12.));
#3734=CARTESIAN_POINT('',(-89.7997772825746,-5.99999999999999,12.));
#3735=CARTESIAN_POINT('',(-21.,-6.,12.));
#3736=CARTESIAN_POINT('',(-89.5382302589158,-9.10523597175682,12.));
#3737=CARTESIAN_POINT('Origin',(0.,0.,12.));
#3738=CARTESIAN_POINT('',(-52.6544807884512,-72.9897640282432,12.));
#3739=CARTESIAN_POINT('Origin',(-86.6025403784438,-50.,12.));
#3740=CARTESIAN_POINT('',(-50.096041063994,-74.7688883808943,12.));
#3741=CARTESIAN_POINT('Origin',(0.,0.,12.));
#3742=CARTESIAN_POINT('',(-26.1961524227066,-33.3730669589464,12.));
#3743=CARTESIAN_POINT('',(-30.1961524227066,-40.3012701892219,12.));
#3744=CARTESIAN_POINT('',(-15.8038475772934,-39.3730669589464,12.));
#3745=CARTESIAN_POINT('Origin',(-21.,-36.3730669589464,12.));
#3746=CARTESIAN_POINT('',(-39.7037362185807,-80.7688883808943,12.));
#3747=CARTESIAN_POINT('',(-5.30384757729338,-21.1865334794732,12.));
#3748=CARTESIAN_POINT('Origin',(0.,0.,12.));
#3749=CARTESIAN_POINT('Origin',(-1.83697019872103E-14,-100.,6.));
#3750=CARTESIAN_POINT('',(36.8837494704646,-82.095,0.));
#3751=CARTESIAN_POINT('',(36.8837494704646,-82.095,6.));
#3752=CARTESIAN_POINT('',(-36.8837494704647,-82.095,0.));
#3753=CARTESIAN_POINT('',(-36.8837494704647,-82.095,6.));
#3754=CARTESIAN_POINT('Origin',(-1.83697019872103E-14,-100.,0.));
#3755=CARTESIAN_POINT('Origin',(-86.6025403784439,50.,6.));
#3756=CARTESIAN_POINT('',(-89.5382302589158,9.10523597175678,0.));
#3757=CARTESIAN_POINT('',(-89.5382302589158,9.10523597175678,6.));
#3758=CARTESIAN_POINT('',(-52.6544807884512,72.9897640282432,0.));
#3759=CARTESIAN_POINT('',(-52.6544807884512,72.9897640282432,6.));
#3760=CARTESIAN_POINT('Origin',(-86.6025403784439,50.,0.));
#3761=CARTESIAN_POINT('Origin',(86.6025403784439,50.,6.));
#3762=CARTESIAN_POINT('',(52.6544807884512,72.9897640282432,0.));
#3763=CARTESIAN_POINT('',(52.6544807884512,72.9897640282432,6.));
#3764=CARTESIAN_POINT('',(89.5382302589158,9.10523597175678,0.));
#3765=CARTESIAN_POINT('',(89.5382302589158,9.10523597175678,6.));
#3766=CARTESIAN_POINT('Origin',(86.6025403784439,50.,0.));
#3767=CARTESIAN_POINT('Origin',(6.12323399573677E-15,100.,6.));
#3768=CARTESIAN_POINT('',(-36.8837494704646,82.095,0.));
#3769=CARTESIAN_POINT('',(-36.8837494704646,82.095,6.));
#3770=CARTESIAN_POINT('',(36.8837494704646,82.095,0.));
#3771=CARTESIAN_POINT('',(36.8837494704646,82.095,6.));
#3772=CARTESIAN_POINT('Origin',(6.12323399573677E-15,100.,0.));
#3773=CARTESIAN_POINT('Origin',(-86.6025403784438,-50.,6.));
#3774=CARTESIAN_POINT('',(-52.6544807884512,-72.9897640282432,0.));
#3775=CARTESIAN_POINT('',(-52.6544807884512,-72.9897640282432,6.));
#3776=CARTESIAN_POINT('',(-89.5382302589158,-9.10523597175679,0.));
#3777=CARTESIAN_POINT('',(-89.5382302589158,-9.10523597175679,6.));
#3778=CARTESIAN_POINT('Origin',(-86.6025403784438,-50.,0.));
#3779=CARTESIAN_POINT('Origin',(86.6025403784438,-50.,6.));
#3780=CARTESIAN_POINT('',(52.6544807884511,-72.9897640282432,0.));
#3781=CARTESIAN_POINT('',(52.6544807884511,-72.9897640282432,6.));
#3782=CARTESIAN_POINT('',(89.5382302589158,-9.10523597175683,0.));
#3783=CARTESIAN_POINT('Origin',(86.6025403784438,-50.,0.));
#3784=CARTESIAN_POINT('',(89.5382302589158,-9.10523597175683,6.));
#3785=CARTESIAN_POINT('Origin',(0.,0.,0.));
#3786=CARTESIAN_POINT('',(-39.7037362185807,-80.7688883808943,0.));
#3787=CARTESIAN_POINT('',(-39.7037362185807,-80.7688883808943,0.));
#3788=CARTESIAN_POINT('Origin',(0.,0.,0.));
#3789=CARTESIAN_POINT('Origin',(0.,0.,0.));
#3790=CARTESIAN_POINT('',(39.7037362185807,-80.7688883808943,0.));
#3791=CARTESIAN_POINT('Origin',(0.,0.,0.));
#3792=CARTESIAN_POINT('',(39.7037362185807,-80.7688883808943,0.));
#3793=CARTESIAN_POINT('Origin',(0.,0.,0.));
#3794=CARTESIAN_POINT('',(-50.0960410639939,74.7688883808943,0.));
#3795=CARTESIAN_POINT('',(-50.0960410639939,74.7688883808943,0.));
#3796=CARTESIAN_POINT('Origin',(0.,0.,0.));
#3797=CARTESIAN_POINT('Origin',(0.,0.,0.));
#3798=CARTESIAN_POINT('',(89.7997772825746,6.,0.));
#3799=CARTESIAN_POINT('',(89.7997772825746,6.,0.));
#3800=CARTESIAN_POINT('Origin',(0.,0.,0.));
#3801=CARTESIAN_POINT('Origin',(0.,0.,0.));
#3802=CARTESIAN_POINT('',(39.7037362185807,80.7688883808943,0.));
#3803=CARTESIAN_POINT('',(39.7037362185807,80.7688883808943,0.));
#3804=CARTESIAN_POINT('Origin',(0.,0.,0.));
#3805=CARTESIAN_POINT('Origin',(0.,0.,0.));
#3806=CARTESIAN_POINT('',(-89.7997772825746,-5.99999999999999,0.));
#3807=CARTESIAN_POINT('',(-89.7997772825746,-5.99999999999999,0.));
#3808=CARTESIAN_POINT('Origin',(0.,0.,0.));
#3809=CARTESIAN_POINT('Origin',(0.,0.,0.));
#3810=CARTESIAN_POINT('',(-15.8038475772934,-39.3730669589464,0.));
#3811=CARTESIAN_POINT('',(-5.30384757729338,-21.1865334794732,0.));
#3812=CARTESIAN_POINT('',(-26.1961524227066,-33.3730669589464,0.));
#3813=CARTESIAN_POINT('Origin',(-21.,-36.3730669589464,0.));
#3814=CARTESIAN_POINT('',(-50.096041063994,-74.7688883808943,0.));
#3815=CARTESIAN_POINT('',(-30.1961524227066,-40.3012701892219,0.));
#3816=CARTESIAN_POINT('Origin',(0.,0.,0.));
#3817=CARTESIAN_POINT('',(-42.,-5.99999999999999,0.));
#3818=CARTESIAN_POINT('',(-21.,-6.,0.));
#3819=CARTESIAN_POINT('',(-42.,6.00000000000001,0.));
#3820=CARTESIAN_POINT('Origin',(-42.,5.14351655641888E-15,0.));
#3821=CARTESIAN_POINT('',(-89.7997772825746,6.00000000000001,0.));
#3822=CARTESIAN_POINT('',(-50.,6.00000000000001,0.));
#3823=CARTESIAN_POINT('Origin',(0.,0.,0.));
#3824=CARTESIAN_POINT('',(-26.1961524227066,33.3730669589464,0.));
#3825=CARTESIAN_POINT('',(-15.6961524227066,15.1865334794732,0.));
#3826=CARTESIAN_POINT('',(-15.8038475772934,39.3730669589464,0.));
#3827=CARTESIAN_POINT('Origin',(-21.,36.3730669589464,0.));
#3828=CARTESIAN_POINT('',(-39.7037362185806,80.7688883808943,0.));
#3829=CARTESIAN_POINT('',(-19.8038475772934,46.3012701892219,0.));
#3830=CARTESIAN_POINT('Origin',(0.,0.,0.));
#3831=CARTESIAN_POINT('',(15.8038475772934,39.3730669589464,0.));
#3832=CARTESIAN_POINT('',(5.30384757729338,21.1865334794732,1.11022302462516E-15));
#3833=CARTESIAN_POINT('',(26.1961524227066,33.3730669589464,0.));
#3834=CARTESIAN_POINT('Origin',(21.,36.3730669589464,0.));
#3835=CARTESIAN_POINT('',(50.0960410639939,74.7688883808943,0.));
#3836=CARTESIAN_POINT('',(30.1961524227066,40.3012701892219,0.));
#3837=CARTESIAN_POINT('Origin',(0.,0.,0.));
#3838=CARTESIAN_POINT('',(42.,6.,0.));
#3839=CARTESIAN_POINT('',(21.,6.,0.));
#3840=CARTESIAN_POINT('',(42.,-6.,0.));
#3841=CARTESIAN_POINT('Origin',(42.,0.,0.));
#3842=CARTESIAN_POINT('',(89.7997772825746,-6.,0.));
#3843=CARTESIAN_POINT('',(50.,-6.,0.));
#3844=CARTESIAN_POINT('Origin',(0.,0.,0.));
#3845=CARTESIAN_POINT('',(50.0960410639939,-74.7688883808943,0.));
#3846=CARTESIAN_POINT('Origin',(0.,0.,0.));
#3847=CARTESIAN_POINT('',(26.1961524227066,-33.3730669589464,0.));
#3848=CARTESIAN_POINT('',(15.6961524227066,-15.1865334794732,0.));
#3849=CARTESIAN_POINT('',(15.8038475772934,-39.3730669589464,0.));
#3850=CARTESIAN_POINT('Origin',(21.,-36.3730669589464,0.));
#3851=CARTESIAN_POINT('',(19.8038475772934,-46.3012701892219,1.11022302462516E-15));
#3852=CARTESIAN_POINT('Origin',(0.,0.,0.));
#3853=CARTESIAN_POINT('',(89.7997772825746,-6.,0.));
#3854=CARTESIAN_POINT('Origin',(0.,0.,0.));
#3855=CARTESIAN_POINT('',(50.0960410639939,-74.7688883808943,0.));
#3856=CARTESIAN_POINT('Origin',(44.8038475772934,-89.6025403784439,12.));
#3857=CARTESIAN_POINT('',(15.8038475772934,-39.3730669589464,12.));
#3858=CARTESIAN_POINT('Origin',(26.1961524227066,-33.3730669589464,12.));
#3859=CARTESIAN_POINT('',(26.1961524227066,-33.3730669589464,12.));
#3860=CARTESIAN_POINT('Origin',(21.,-36.3730669589464,12.));
#3861=CARTESIAN_POINT('Origin',(-55.1961524227066,-83.6025403784438,12.));
#3862=CARTESIAN_POINT('',(-50.096041063994,-74.7688883808943,0.));
#3863=CARTESIAN_POINT('',(-26.1961524227066,-33.3730669589464,12.));
#3864=CARTESIAN_POINT('Origin',(-15.8038475772934,-39.3730669589464,12.));
#3865=CARTESIAN_POINT('',(-15.8038475772934,-39.3730669589464,12.));
#3866=CARTESIAN_POINT('Origin',(-21.,-36.3730669589464,12.));
#3867=CARTESIAN_POINT('Origin',(-100.,6.00000000000001,12.));
#3868=CARTESIAN_POINT('',(-89.7997772825746,6.00000000000001,0.));
#3869=CARTESIAN_POINT('',(-42.,6.00000000000001,12.));
#3870=CARTESIAN_POINT('Origin',(-42.,-5.99999999999999,12.));
#3871=CARTESIAN_POINT('',(-42.,-5.99999999999999,12.));
#3872=CARTESIAN_POINT('Origin',(-42.,5.14351655641888E-15,12.));
#3873=CARTESIAN_POINT('Origin',(0.,0.,0.));
#3874=CARTESIAN_POINT('Origin',(0.,0.,0.));
#3875=CARTESIAN_POINT('Origin',(-44.8038475772934,89.6025403784439,12.));
#3876=CARTESIAN_POINT('',(-39.7037362185806,80.7688883808943,0.));
#3877=CARTESIAN_POINT('',(-15.8038475772934,39.3730669589464,12.));
#3878=CARTESIAN_POINT('Origin',(-26.1961524227066,33.3730669589464,12.));
#3879=CARTESIAN_POINT('',(-26.1961524227066,33.3730669589464,12.));
#3880=CARTESIAN_POINT('Origin',(-21.,36.3730669589464,12.));
#3881=CARTESIAN_POINT('Origin',(55.1961524227066,83.6025403784438,12.));
#3882=CARTESIAN_POINT('',(50.0960410639939,74.7688883808943,0.));
#3883=CARTESIAN_POINT('',(26.1961524227066,33.3730669589464,12.));
#3884=CARTESIAN_POINT('Origin',(15.8038475772934,39.3730669589464,12.));
#3885=CARTESIAN_POINT('',(15.8038475772934,39.3730669589464,12.));
#3886=CARTESIAN_POINT('Origin',(21.,36.3730669589464,12.));
#3887=CARTESIAN_POINT('Origin',(0.,0.,0.));
#3888=CARTESIAN_POINT('Origin',(0.,0.,0.));
#3889=CARTESIAN_POINT('Origin',(100.,-6.,12.));
#3890=CARTESIAN_POINT('',(42.,-6.,12.));
#3891=CARTESIAN_POINT('Origin',(42.,6.,12.));
#3892=CARTESIAN_POINT('',(42.,6.,12.));
#3893=CARTESIAN_POINT('Origin',(42.,0.,12.));
#3894=CARTESIAN_POINT('',(0.,0.,0.));
#3895=CARTESIAN_POINT('Origin',(8.,-1.5,44.));
#3896=CARTESIAN_POINT('',(4.76969600708473,-1.5,32.));
#3897=CARTESIAN_POINT('',(4.76969600708473,-1.5,44.));
#3898=CARTESIAN_POINT('',(4.76969600708473,-1.5,0.));
#3899=CARTESIAN_POINT('',(3.,-1.5,32.));
#3900=CARTESIAN_POINT('',(3.,-1.5,32.));
#3901=CARTESIAN_POINT('',(3.,-1.5,44.));
#3902=CARTESIAN_POINT('',(3.,-1.5,44.));
#3903=CARTESIAN_POINT('',(3.,-1.5,44.));
#3904=CARTESIAN_POINT('Origin',(5.5,0.,44.));
#3905=CARTESIAN_POINT('',(4.76969600708473,1.5,44.));
#3906=CARTESIAN_POINT('Origin',(0.,0.,44.));
#3907=CARTESIAN_POINT('',(3.,1.5,44.));
#3908=CARTESIAN_POINT('',(3.,1.5,44.));
#3909=CARTESIAN_POINT('',(8.,1.5,44.));
#3910=CARTESIAN_POINT('Origin',(3.,1.5,44.));
#3911=CARTESIAN_POINT('',(4.76969600708473,1.5,32.));
#3912=CARTESIAN_POINT('',(4.76969600708473,1.5,0.));
#3913=CARTESIAN_POINT('',(3.,1.5,32.));
#3914=CARTESIAN_POINT('',(3.,1.5,44.));
#3915=CARTESIAN_POINT('',(8.,1.5,32.));
#3916=CARTESIAN_POINT('Origin',(3.,-1.5,44.));
#3917=CARTESIAN_POINT('',(3.,1.5,32.));
#3918=CARTESIAN_POINT('Origin',(5.5,0.,32.));
#3919=CARTESIAN_POINT('Origin',(0.,0.,32.));
#3920=CARTESIAN_POINT('Origin',(0.,0.,51.));
#3921=CARTESIAN_POINT('',(-4.,-4.89858719658941E-16,50.));
#3922=CARTESIAN_POINT('Origin',(0.,0.,50.));
#3923=CARTESIAN_POINT('',(-4.,-4.89858719658941E-16,52.));
#3924=CARTESIAN_POINT('',(-4.,-4.89858719658941E-16,51.));
#3925=CARTESIAN_POINT('Origin',(0.,0.,52.));
#3926=CARTESIAN_POINT('Origin',(8.,0.,50.));
#3927=CARTESIAN_POINT('',(-5.,6.12323399573677E-16,50.));
#3928=CARTESIAN_POINT('Origin',(0.,0.,50.));
#3929=CARTESIAN_POINT('Origin',(4.,0.,52.));
#3930=CARTESIAN_POINT('',(-5.,-6.12323399573677E-16,52.));
#3931=CARTESIAN_POINT('Origin',(0.,0.,52.));
#3932=CARTESIAN_POINT('Origin',(0.,0.,0.));
#3933=CARTESIAN_POINT('',(-5.,-6.12323399573677E-16,53.));
#3934=CARTESIAN_POINT('Origin',(0.,0.,53.));
#3935=CARTESIAN_POINT('',(-5.,-6.12323399573677E-16,0.));
#3936=CARTESIAN_POINT('Origin',(0.,0.,0.));
#3937=CARTESIAN_POINT('',(-8.,-9.79717439317883E-16,0.));
#3938=CARTESIAN_POINT('Origin',(0.,0.,0.));
#3939=CARTESIAN_POINT('',(-5.,-6.12323399573677E-16,0.));
#3940=CARTESIAN_POINT('Origin',(0.,0.,0.));
#3941=CARTESIAN_POINT('Origin',(0.,0.,-4.));
#3942=CARTESIAN_POINT('',(-8.,-9.79717439317883E-16,-4.));
#3943=CARTESIAN_POINT('',(-8.,-9.79717439317883E-16,-4.));
#3944=CARTESIAN_POINT('Origin',(0.,0.,-4.));
#3945=CARTESIAN_POINT('Origin',(0.,0.,-4.));
#3946=CARTESIAN_POINT('Origin',(0.,0.,0.));
#3947=CARTESIAN_POINT('',(-5.,-6.12323399573677E-16,0.));
#3948=CARTESIAN_POINT('Origin',(0.,0.,53.));
#3949=CARTESIAN_POINT('',(0.,0.,0.));
#3950=CARTESIAN_POINT('Origin',(6.,1.5,32.));
#3951=CARTESIAN_POINT('',(6.,1.5,32.));
#3952=CARTESIAN_POINT('',(3.,1.5,32.));
#3953=CARTESIAN_POINT('',(6.,1.5,32.));
#3954=CARTESIAN_POINT('',(3.,1.5,44.));
#3955=CARTESIAN_POINT('',(3.,1.5,32.));
#3956=CARTESIAN_POINT('',(6.,1.5,44.));
#3957=CARTESIAN_POINT('',(6.,1.5,44.));
#3958=CARTESIAN_POINT('',(6.,1.5,32.));
#3959=CARTESIAN_POINT('Origin',(6.,-1.5,32.));
#3960=CARTESIAN_POINT('',(6.,-1.5,32.));
#3961=CARTESIAN_POINT('',(6.,-1.5,32.));
#3962=CARTESIAN_POINT('',(6.,-1.5,44.));
#3963=CARTESIAN_POINT('',(6.,-1.5,44.));
#3964=CARTESIAN_POINT('',(6.,-1.5,32.));
#3965=CARTESIAN_POINT('Origin',(3.,-1.5,32.));
#3966=CARTESIAN_POINT('',(3.,-1.5,32.));
#3967=CARTESIAN_POINT('',(3.,-1.5,32.));
#3968=CARTESIAN_POINT('',(3.,-1.5,44.));
#3969=CARTESIAN_POINT('',(3.,-1.5,44.));
#3970=CARTESIAN_POINT('',(3.,-1.5,32.));
#3971=CARTESIAN_POINT('Origin',(3.,1.5,32.));
#3972=CARTESIAN_POINT('',(3.,1.5,32.));
#3973=CARTESIAN_POINT('',(3.,1.5,44.));
#3974=CARTESIAN_POINT('Origin',(4.5,0.,44.));
#3975=CARTESIAN_POINT('Origin',(4.5,0.,32.));
#3976=CARTESIAN_POINT('',(0.,0.,0.));
#3977=CARTESIAN_POINT('Origin',(0.,0.,20.));
#3978=CARTESIAN_POINT('',(-7.,-8.57252759403147E-16,20.));
#3979=CARTESIAN_POINT('Origin',(0.,0.,20.));
#3980=CARTESIAN_POINT('',(-5.,-6.12323399573677E-16,20.));
#3981=CARTESIAN_POINT('Origin',(0.,0.,20.));
#3982=CARTESIAN_POINT('Origin',(0.,0.,8.));
#3983=CARTESIAN_POINT('',(-7.,-8.57252759403147E-16,8.));
#3984=CARTESIAN_POINT('Origin',(0.,0.,8.));
#3985=CARTESIAN_POINT('',(-5.,6.12323399573677E-16,8.));
#3986=CARTESIAN_POINT('Origin',(0.,0.,8.));
#3987=CARTESIAN_POINT('Origin',(0.,0.,8.));
#3988=CARTESIAN_POINT('',(-7.,-8.57252759403147E-16,8.));
#3989=CARTESIAN_POINT('Origin',(0.,0.,0.));
#3990=CARTESIAN_POINT('',(-5.,-6.12323399573677E-16,0.));
#3991=CARTESIAN_POINT('',(-5.,-6.12323399573677E-16,0.));
#3992=CARTESIAN_POINT('Origin',(0.,0.,0.));
#3993=CARTESIAN_POINT('Origin',(0.,0.,33.));
#3994=CARTESIAN_POINT('',(-4.,-4.89858719658941E-16,32.));
#3995=CARTESIAN_POINT('Origin',(0.,0.,32.));
#3996=CARTESIAN_POINT('',(-4.,-4.89858719658941E-16,34.));
#3997=CARTESIAN_POINT('',(-4.,-4.89858719658941E-16,33.));
#3998=CARTESIAN_POINT('Origin',(0.,0.,34.));
#3999=CARTESIAN_POINT('Origin',(8.,0.,32.));
#4000=CARTESIAN_POINT('',(-5.,6.12323399573677E-16,32.));
#4001=CARTESIAN_POINT('Origin',(0.,0.,32.));
#4002=CARTESIAN_POINT('Origin',(4.,0.,34.));
#4003=CARTESIAN_POINT('',(-5.,-6.12323399573677E-16,34.));
#4004=CARTESIAN_POINT('Origin',(0.,0.,34.));
#4005=CARTESIAN_POINT('Origin',(0.,0.,0.));
#4006=CARTESIAN_POINT('',(-5.,-6.12323399573677E-16,35.));
#4007=CARTESIAN_POINT('Origin',(0.,0.,35.));
#4008=CARTESIAN_POINT('',(-5.,-6.12323399573677E-16,0.));
#4009=CARTESIAN_POINT('Origin',(0.,0.,0.));
#4010=CARTESIAN_POINT('',(-8.,-9.79717439317883E-16,0.));
#4011=CARTESIAN_POINT('Origin',(0.,0.,0.));
#4012=CARTESIAN_POINT('Origin',(0.,0.,-1.));
#4013=CARTESIAN_POINT('',(-8.,-9.79717439317883E-16,-1.));
#4014=CARTESIAN_POINT('',(-8.,-9.79717439317883E-16,-1.));
#4015=CARTESIAN_POINT('Origin',(0.,0.,-1.));
#4016=CARTESIAN_POINT('Origin',(0.,0.,-1.));
#4017=CARTESIAN_POINT('Origin',(0.,0.,0.));
#4018=CARTESIAN_POINT('',(-5.,-6.12323399573677E-16,0.));
#4019=CARTESIAN_POINT('Origin',(0.,0.,35.));
#4020=CARTESIAN_POINT('',(0.,0.,0.));
#4021=CARTESIAN_POINT('Origin',(0.,0.,0.));
#4022=CARTESIAN_POINT('',(-5.,-6.12323399573677E-16,8.));
#4023=CARTESIAN_POINT('Origin',(0.,0.,8.));
#4024=CARTESIAN_POINT('',(-5.,-6.12323399573677E-16,0.));
#4025=CARTESIAN_POINT('',(-5.,-6.12323399573677E-16,0.));
#4026=CARTESIAN_POINT('Origin',(0.,0.,0.));
#4027=CARTESIAN_POINT('Origin',(0.,0.,0.));
#4028=CARTESIAN_POINT('',(-7.,-8.57252759403147E-16,8.));
#4029=CARTESIAN_POINT('Origin',(0.,0.,8.));
#4030=CARTESIAN_POINT('',(-7.,-8.57252759403147E-16,0.));
#4031=CARTESIAN_POINT('',(-7.,-8.57252759403147E-16,0.));
#4032=CARTESIAN_POINT('Origin',(0.,0.,0.));
#4033=CARTESIAN_POINT('Origin',(0.,0.,8.));
#4034=CARTESIAN_POINT('Origin',(0.,0.,0.));
#4035=CARTESIAN_POINT('',(0.,0.,0.));
#4036=CARTESIAN_POINT('Origin',(0.,0.,0.));
#4037=CARTESIAN_POINT('',(-5.,-6.12323399573677E-16,20.));
#4038=CARTESIAN_POINT('Origin',(0.,0.,20.));
#4039=CARTESIAN_POINT('',(-5.,-6.12323399573677E-16,0.));
#4040=CARTESIAN_POINT('',(-5.,-6.12323399573677E-16,0.));
#4041=CARTESIAN_POINT('Origin',(0.,0.,0.));
#4042=CARTESIAN_POINT('Origin',(0.,0.,0.));
#4043=CARTESIAN_POINT('',(-7.,-8.57252759403147E-16,20.));
#4044=CARTESIAN_POINT('Origin',(0.,0.,20.));
#4045=CARTESIAN_POINT('',(-7.,-8.57252759403147E-16,0.));
#4046=CARTESIAN_POINT('',(-7.,-8.57252759403147E-16,0.));
#4047=CARTESIAN_POINT('Origin',(0.,0.,0.));
#4048=CARTESIAN_POINT('Origin',(0.,0.,20.));
#4049=CARTESIAN_POINT('Origin',(0.,0.,0.));
#4050=CARTESIAN_POINT('',(0.,0.,0.));
#4051=CARTESIAN_POINT('Origin',(0.,0.,0.));
#4052=CARTESIAN_POINT('',(-5.,-6.12323399573677E-16,4.));
#4053=CARTESIAN_POINT('Origin',(0.,0.,4.));
#4054=CARTESIAN_POINT('',(-5.,-6.12323399573677E-16,0.));
#4055=CARTESIAN_POINT('',(-5.,-6.12323399573677E-16,0.));
#4056=CARTESIAN_POINT('Origin',(0.,0.,0.));
#4057=CARTESIAN_POINT('Origin',(0.,0.,0.));
#4058=CARTESIAN_POINT('',(-7.,-8.57252759403147E-16,4.));
#4059=CARTESIAN_POINT('Origin',(0.,0.,4.));
#4060=CARTESIAN_POINT('',(-7.,-8.57252759403147E-16,0.));
#4061=CARTESIAN_POINT('',(-7.,-8.57252759403147E-16,0.));
#4062=CARTESIAN_POINT('Origin',(0.,0.,0.));
#4063=CARTESIAN_POINT('Origin',(0.,0.,4.));
#4064=CARTESIAN_POINT('Origin',(0.,0.,0.));
#4065=CARTESIAN_POINT('',(0.,0.,0.));
#4066=CARTESIAN_POINT('Origin',(0.,0.,0.));
#4067=CARTESIAN_POINT('',(-5.,-6.12323399573677E-16,2.));
#4068=CARTESIAN_POINT('Origin',(0.,0.,2.));
#4069=CARTESIAN_POINT('',(-5.,-6.12323399573677E-16,0.));
#4070=CARTESIAN_POINT('',(-5.,-6.12323399573677E-16,0.));
#4071=CARTESIAN_POINT('Origin',(0.,0.,0.));
#4072=CARTESIAN_POINT('Origin',(0.,0.,0.));
#4073=CARTESIAN_POINT('',(-10.,-1.22464679914735E-15,2.));
#4074=CARTESIAN_POINT('Origin',(0.,0.,2.));
#4075=CARTESIAN_POINT('',(-10.,-1.22464679914735E-15,0.));
#4076=CARTESIAN_POINT('',(-10.,-1.22464679914735E-15,0.));
#4077=CARTESIAN_POINT('Origin',(0.,0.,0.));
#4078=CARTESIAN_POINT('Origin',(0.,0.,2.));
#4079=CARTESIAN_POINT('Origin',(0.,0.,0.));
#4080=CARTESIAN_POINT('',(0.,0.,0.));
#4081=CARTESIAN_POINT('Origin',(-1.,0.,1.));
#4082=CARTESIAN_POINT('',(-1.,3.87298334620742,0.));
#4083=CARTESIAN_POINT('',(-1.,3.87298334620742,1.));
#4084=CARTESIAN_POINT('',(-1.,3.87298334620742,0.));
#4085=CARTESIAN_POINT('',(-1.,7.93725393319377,0.));
#4086=CARTESIAN_POINT('',(-1.,0.,0.));
#4087=CARTESIAN_POINT('',(-1.,7.93725393319377,1.));
#4088=CARTESIAN_POINT('',(-1.,7.93725393319377,0.));
#4089=CARTESIAN_POINT('',(-1.,0.,1.));
#4090=CARTESIAN_POINT('Origin',(1.,16.,1.));
#4091=CARTESIAN_POINT('',(1.,3.87298334620742,1.));
#4092=CARTESIAN_POINT('',(1.,3.87298334620742,0.));
#4093=CARTESIAN_POINT('',(1.,3.87298334620742,0.));
#4094=CARTESIAN_POINT('',(1.,7.93725393319377,1.));
#4095=CARTESIAN_POINT('',(1.,8.,1.));
#4096=CARTESIAN_POINT('',(1.,7.93725393319377,0.));
#4097=CARTESIAN_POINT('',(1.,7.93725393319377,0.));
#4098=CARTESIAN_POINT('',(1.,8.,0.));
#4099=CARTESIAN_POINT('Origin',(0.,0.,0.));
#4100=CARTESIAN_POINT('Origin',(0.,0.,0.));
#4101=CARTESIAN_POINT('Origin',(0.,0.,0.));
#4102=CARTESIAN_POINT('Origin',(0.,0.,0.));
#4103=CARTESIAN_POINT('Origin',(0.,0.,1.));
#4104=CARTESIAN_POINT('Origin',(0.,0.,0.));
#4105=CARTESIAN_POINT('Origin',(0.,0.,1.));
#4106=CARTESIAN_POINT('Origin',(0.,0.,1.));
#4107=CARTESIAN_POINT('',(0.,0.,0.));
#4108=CARTESIAN_POINT('',(0.,0.,0.));
#4109=CARTESIAN_POINT('',(100.,0.,32.));
#4110=CARTESIAN_POINT('',(100.,0.,0.));
#4111=CARTESIAN_POINT('',(100.,0.,0.));
#4112=CARTESIAN_POINT('',(50.,0.,12.));
#4113=CARTESIAN_POINT('',(0.,0.,1.));
#4114=CARTESIAN_POINT('',(100.,0.,1.));
#4115=CARTESIAN_POINT('',(100.,0.,12.));
#4116=CARTESIAN_POINT('',(100.,0.,46.));
#4117=CARTESIAN_POINT('',(0.,0.,10.));
#4118=CARTESIAN_POINT('',(0.,0.,-2.));
#4119=CARTESIAN_POINT('',(100.,0.,10.));
#4120=CARTESIAN_POINT('',(100.,0.,44.));
#4121=CARTESIAN_POINT('',(0.,0.,-3.));
#4122=CARTESIAN_POINT('',(100.,0.,51.));
#4123=CARTESIAN_POINT('',(50.,0.,45.));
#4124=UNCERTAINTY_MEASURE_WITH_UNIT(LENGTH_MEASURE(0.01),#4150,
'DISTANCE_ACCURACY_VALUE',
'Maximum model space distance between geometric entities at asserted c
onnectivities');
#4125=UNCERTAINTY_MEASURE_WITH_UNIT(LENGTH_MEASURE(0.01),#4150,
'DISTANCE_ACCURACY_VALUE',
'Maximum model space distance between geometric entities at asserted c
onnectivities');
#4126=UNCERTAINTY_MEASURE_WITH_UNIT(LENGTH_MEASURE(0.01),#4150,
'DISTANCE_ACCURACY_VALUE',
'Maximum model space distance between geometric entities at asserted c
onnectivities');
#4127=UNCERTAINTY_MEASURE_WITH_UNIT(LENGTH_MEASURE(0.01),#4150,
'DISTANCE_ACCURACY_VALUE',
'Maximum model space distance between geometric entities at asserted c
onnectivities');
#4128=UNCERTAINTY_MEASURE_WITH_UNIT(LENGTH_MEASURE(0.01),#4150,
'DISTANCE_ACCURACY_VALUE',
'Maximum model space distance between geometric entities at asserted c
onnectivities');
#4129=UNCERTAINTY_MEASURE_WITH_UNIT(LENGTH_MEASURE(0.01),#4150,
'DISTANCE_ACCURACY_VALUE',
'Maximum model space distance between geometric entities at asserted c
onnectivities');
#4130=UNCERTAINTY_MEASURE_WITH_UNIT(LENGTH_MEASURE(0.01),#4150,
'DISTANCE_ACCURACY_VALUE',
'Maximum model space distance between geometric entities at asserted c
onnectivities');
#4131=UNCERTAINTY_MEASURE_WITH_UNIT(LENGTH_MEASURE(0.01),#4150,
'DISTANCE_ACCURACY_VALUE',
'Maximum model space distance between geometric entities at asserted c
onnectivities');
#4132=UNCERTAINTY_MEASURE_WITH_UNIT(LENGTH_MEASURE(0.01),#4150,
'DISTANCE_ACCURACY_VALUE',
'Maximum model space distance between geometric entities at asserted c
onnectivities');
#4133=UNCERTAINTY_MEASURE_WITH_UNIT(LENGTH_MEASURE(0.01),#4150,
'DISTANCE_ACCURACY_VALUE',
'Maximum model space distance between geometric entities at asserted c
onnectivities');
#4134=UNCERTAINTY_MEASURE_WITH_UNIT(LENGTH_MEASURE(0.01),#4150,
'DISTANCE_ACCURACY_VALUE',
'Maximum model space distance between geometric entities at asserted c
onnectivities');
#4135=UNCERTAINTY_MEASURE_WITH_UNIT(LENGTH_MEASURE(0.01),#4150,
'DISTANCE_ACCURACY_VALUE',
'Maximum model space distance between geometric entities at asserted c
onnectivities');
#4136=UNCERTAINTY_MEASURE_WITH_UNIT(LENGTH_MEASURE(0.01),#4150,
'DISTANCE_ACCURACY_VALUE',
'Maximum model space distance between geometric entities at asserted c
onnectivities');
#4137=(
GEOMETRIC_REPRESENTATION_CONTEXT(3)
GLOBAL_UNCERTAINTY_ASSIGNED_CONTEXT((#4124))
GLOBAL_UNIT_ASSIGNED_CONTEXT((#4150,#4152,#4153))
REPRESENTATION_CONTEXT('','3D')
);
#4138=(
GEOMETRIC_REPRESENTATION_CONTEXT(3)
GLOBAL_UNCERTAINTY_ASSIGNED_CONTEXT((#4125))
GLOBAL_UNIT_ASSIGNED_CONTEXT((#4150,#4152,#4153))
REPRESENTATION_CONTEXT('','3D')
);
#4139=(
GEOMETRIC_REPRESENTATION_CONTEXT(3)
GLOBAL_UNCERTAINTY_ASSIGNED_CONTEXT((#4126))
GLOBAL_UNIT_ASSIGNED_CONTEXT((#4150,#4152,#4153))
REPRESENTATION_CONTEXT('','3D')
);
#4140=(
GEOMETRIC_REPRESENTATION_CONTEXT(3)
GLOBAL_UNCERTAINTY_ASSIGNED_CONTEXT((#4127))
GLOBAL_UNIT_ASSIGNED_CONTEXT((#4150,#4152,#4153))
REPRESENTATION_CONTEXT('','3D')
);
#4141=(
GEOMETRIC_REPRESENTATION_CONTEXT(3)
GLOBAL_UNCERTAINTY_ASSIGNED_CONTEXT((#4128))
GLOBAL_UNIT_ASSIGNED_CONTEXT((#4150,#4152,#4153))
REPRESENTATION_CONTEXT('','3D')
);
#4142=(
GEOMETRIC_REPRESENTATION_CONTEXT(3)
GLOBAL_UNCERTAINTY_ASSIGNED_CONTEXT((#4129))
GLOBAL_UNIT_ASSIGNED_CONTEXT((#4150,#4152,#4153))
REPRESENTATION_CONTEXT('','3D')
);
#4143=(
GEOMETRIC_REPRESENTATION_CONTEXT(3)
GLOBAL_UNCERTAINTY_ASSIGNED_CONTEXT((#4130))
GLOBAL_UNIT_ASSIGNED_CONTEXT((#4150,#4152,#4153))
REPRESENTATION_CONTEXT('','3D')
);
#4144=(
GEOMETRIC_REPRESENTATION_CONTEXT(3)
GLOBAL_UNCERTAINTY_ASSIGNED_CONTEXT((#4131))
GLOBAL_UNIT_ASSIGNED_CONTEXT((#4150,#4152,#4153))
REPRESENTATION_CONTEXT('','3D')
);
#4145=(
GEOMETRIC_REPRESENTATION_CONTEXT(3)
GLOBAL_UNCERTAINTY_ASSIGNED_CONTEXT((#4132))
GLOBAL_UNIT_ASSIGNED_CONTEXT((#4150,#4152,#4153))
REPRESENTATION_CONTEXT('','3D')
);
#4146=(
GEOMETRIC_REPRESENTATION_CONTEXT(3)
GLOBAL_UNCERTAINTY_ASSIGNED_CONTEXT((#4133))
GLOBAL_UNIT_ASSIGNED_CONTEXT((#4150,#4152,#4153))
REPRESENTATION_CONTEXT('','3D')
);
#4147=(
GEOMETRIC_REPRESENTATION_CONTEXT(3)
GLOBAL_UNCERTAINTY_ASSIGNED_CONTEXT((#4134))
GLOBAL_UNIT_ASSIGNED_CONTEXT((#4150,#4152,#4153))
REPRESENTATION_CONTEXT('','3D')
);
#4148=(
GEOMETRIC_REPRESENTATION_CONTEXT(3)
GLOBAL_UNCERTAINTY_ASSIGNED_CONTEXT((#4135))
GLOBAL_UNIT_ASSIGNED_CONTEXT((#4150,#4152,#4153))
REPRESENTATION_CONTEXT('','3D')
);
#4149=(
GEOMETRIC_REPRESENTATION_CONTEXT(3)
GLOBAL_UNCERTAINTY_ASSIGNED_CONTEXT((#4136))
GLOBAL_UNIT_ASSIGNED_CONTEXT((#4150,#4152,#4153))
REPRESENTATION_CONTEXT('','3D')
);
#4150=(
LENGTH_UNIT()
NAMED_UNIT(*)
SI_UNIT(.MILLI.,.METRE.)
);
#4151=(
LENGTH_UNIT()
NAMED_UNIT(*)
SI_UNIT($,.METRE.)
);
#4152=(
NAMED_UNIT(*)
PLANE_ANGLE_UNIT()
SI_UNIT($,.RADIAN.)
);
#4153=(
NAMED_UNIT(*)
SI_UNIT($,.STERADIAN.)
SOLID_ANGLE_UNIT()
);
#4154=SHAPE_DEFINITION_REPRESENTATION(#4166,#4195);
#4155=SHAPE_DEFINITION_REPRESENTATION(#4167,#4196);
#4156=SHAPE_DEFINITION_REPRESENTATION(#4168,#4197);
#4157=SHAPE_DEFINITION_REPRESENTATION(#4169,#4198);
#4158=SHAPE_DEFINITION_REPRESENTATION(#4170,#4199);
#4159=SHAPE_DEFINITION_REPRESENTATION(#4171,#4200);
#4160=SHAPE_DEFINITION_REPRESENTATION(#4172,#4201);
#4161=SHAPE_DEFINITION_REPRESENTATION(#4173,#4202);
#4162=SHAPE_DEFINITION_REPRESENTATION(#4174,#4203);
#4163=SHAPE_DEFINITION_REPRESENTATION(#4175,#4204);
#4164=SHAPE_DEFINITION_REPRESENTATION(#4176,#4205);
#4165=SHAPE_DEFINITION_REPRESENTATION(#4177,#4206);
#4166=PRODUCT_DEFINITION_SHAPE('',$,#4208);
#4167=PRODUCT_DEFINITION_SHAPE('',$,#4209);
#4168=PRODUCT_DEFINITION_SHAPE('',$,#4210);
#4169=PRODUCT_DEFINITION_SHAPE('',$,#4211);
#4170=PRODUCT_DEFINITION_SHAPE('',$,#4212);
#4171=PRODUCT_DEFINITION_SHAPE('',$,#4213);
#4172=PRODUCT_DEFINITION_SHAPE('',$,#4214);
#4173=PRODUCT_DEFINITION_SHAPE('',$,#4215);
#4174=PRODUCT_DEFINITION_SHAPE('',$,#4216);
#4175=PRODUCT_DEFINITION_SHAPE('',$,#4217);
#4176=PRODUCT_DEFINITION_SHAPE('',$,#4218);
#4177=PRODUCT_DEFINITION_SHAPE('',$,#4219);
#4178=PRODUCT_DEFINITION_SHAPE($,$,#62);
#4179=PRODUCT_DEFINITION_SHAPE($,$,#63);
#4180=PRODUCT_DEFINITION_SHAPE($,$,#64);
#4181=PRODUCT_DEFINITION_SHAPE($,$,#65);
#4182=PRODUCT_DEFINITION_SHAPE($,$,#66);
#4183=PRODUCT_DEFINITION_SHAPE($,$,#67);
#4184=PRODUCT_DEFINITION_SHAPE($,$,#68);
#4185=PRODUCT_DEFINITION_SHAPE($,$,#69);
#4186=PRODUCT_DEFINITION_SHAPE($,$,#70);
#4187=PRODUCT_DEFINITION_SHAPE($,$,#71);
#4188=PRODUCT_DEFINITION_SHAPE($,$,#72);
#4189=PRODUCT_DEFINITION_SHAPE($,$,#73);
#4190=PRODUCT_DEFINITION_SHAPE($,$,#74);
#4191=PRODUCT_DEFINITION_SHAPE($,$,#75);
#4192=PRODUCT_DEFINITION_SHAPE($,$,#76);
#4193=PRODUCT_DEFINITION_SHAPE($,$,#77);
#4194=PRODUCT_DEFINITION_SHAPE($,$,#78);
#4195=SHAPE_REPRESENTATION('',(#2428,#2700,#2701,#2702,#2703,#2704,#2705,
#2706,#2707,#2708,#2709,#2710,#2711,#2712,#2713,#2714,#2715,#2716),#4137);
#4196=SHAPE_REPRESENTATION('',(#2429),#4138);
#4197=SHAPE_REPRESENTATION('',(#2454),#4139);
#4198=SHAPE_REPRESENTATION('',(#2502),#4140);
#4199=SHAPE_REPRESENTATION('',(#2595),#4141);
#4200=SHAPE_REPRESENTATION('',(#2620),#4142);
#4201=SHAPE_REPRESENTATION('',(#2627),#4143);
#4202=SHAPE_REPRESENTATION('',(#2653),#4144);
#4203=SHAPE_REPRESENTATION('',(#2662),#4145);
#4204=SHAPE_REPRESENTATION('',(#2671),#4146);
#4205=SHAPE_REPRESENTATION('',(#2680),#4147);
#4206=SHAPE_REPRESENTATION('',(#2689),#4148);
#4207=PRODUCT_DEFINITION_CONTEXT('part definition',#4245,'design');
#4208=PRODUCT_DEFINITION('MAS-207','MAS-207',#4220,#4207);
#4209=PRODUCT_DEFINITION('Base plate','Base plate',#4221,#4207);
#4210=PRODUCT_DEFINITION('Driving rotor','Driving rotor',#4222,#4207);
#4211=PRODUCT_DEFINITION('Indexing starwheel','Indexing starwheel',#4223,
#4207);
#4212=PRODUCT_DEFINITION('Output shaft','Output shaft',#4224,#4207);
#4213=PRODUCT_DEFINITION('Drive key','Drive key',#4225,#4207);
#4214=PRODUCT_DEFINITION('Drive pin','Drive pin',#4226,#4207);
#4215=PRODUCT_DEFINITION('Pivot bushing','Pivot bushing',#4227,#4207);
#4216=PRODUCT_DEFINITION('Wheel spacer','Wheel spacer',#4228,#4207);
#4217=PRODUCT_DEFINITION('Retaining spacer','Retaining spacer',#4229,#4207);
#4218=PRODUCT_DEFINITION('Pivot washer','Pivot washer',#4230,#4207);
#4219=PRODUCT_DEFINITION('Pivot retaining ring','Pivot retaining ring',
#4231,#4207);
#4220=PRODUCT_DEFINITION_FORMATION('',$,#4247);
#4221=PRODUCT_DEFINITION_FORMATION('',$,#4248);
#4222=PRODUCT_DEFINITION_FORMATION('',$,#4249);
#4223=PRODUCT_DEFINITION_FORMATION('',$,#4250);
#4224=PRODUCT_DEFINITION_FORMATION('',$,#4251);
#4225=PRODUCT_DEFINITION_FORMATION('',$,#4252);
#4226=PRODUCT_DEFINITION_FORMATION('',$,#4253);
#4227=PRODUCT_DEFINITION_FORMATION('',$,#4254);
#4228=PRODUCT_DEFINITION_FORMATION('',$,#4255);
#4229=PRODUCT_DEFINITION_FORMATION('',$,#4256);
#4230=PRODUCT_DEFINITION_FORMATION('',$,#4257);
#4231=PRODUCT_DEFINITION_FORMATION('',$,#4258);
#4232=PRODUCT_RELATED_PRODUCT_CATEGORY('MAS-207','MAS-207',(#4247));
#4233=PRODUCT_RELATED_PRODUCT_CATEGORY('Base plate','Base plate',(#4248));
#4234=PRODUCT_RELATED_PRODUCT_CATEGORY('Driving rotor','Driving rotor',
(#4249));
#4235=PRODUCT_RELATED_PRODUCT_CATEGORY('Indexing starwheel',
'Indexing starwheel',(#4250));
#4236=PRODUCT_RELATED_PRODUCT_CATEGORY('Output shaft','Output shaft',(#4251));
#4237=PRODUCT_RELATED_PRODUCT_CATEGORY('Drive key','Drive key',(#4252));
#4238=PRODUCT_RELATED_PRODUCT_CATEGORY('Drive pin','Drive pin',(#4253));
#4239=PRODUCT_RELATED_PRODUCT_CATEGORY('Pivot bushing','Pivot bushing',
(#4254));
#4240=PRODUCT_RELATED_PRODUCT_CATEGORY('Wheel spacer','Wheel spacer',(#4255));
#4241=PRODUCT_RELATED_PRODUCT_CATEGORY('Retaining spacer',
'Retaining spacer',(#4256));
#4242=PRODUCT_RELATED_PRODUCT_CATEGORY('Pivot washer','Pivot washer',(#4257));
#4243=PRODUCT_RELATED_PRODUCT_CATEGORY('Pivot retaining ring',
'Pivot retaining ring',(#4258));
#4244=APPLICATION_PROTOCOL_DEFINITION('international standard',
'automotive_design',2009,#4245);
#4245=APPLICATION_CONTEXT(
'Core Data for Automotive Mechanical Design Process');
#4246=PRODUCT_CONTEXT('part definition',#4245,'mechanical');
#4247=PRODUCT('MAS-207','MAS-207',
'Independent six-slot Geneva indexer. Center distance100, drive radius
50, 60degree indexing per input revolution with120degree engagement an
d240degree dwell. Native machined concave locking faces and relieved d
isk; replaceable retained drive pin; keyed output shaft. Geometry traj
ectory checks use calculated indexing positions, not a contact-dynamic
s simulation. No load or production rating assigned.',(#4246));
#4248=PRODUCT('Base plate','Base plate','Base plate',(#4246));
#4249=PRODUCT('Driving rotor','Driving rotor',$,(#4246));
#4250=PRODUCT('Indexing starwheel','Indexing starwheel',$,(#4246));
#4251=PRODUCT('Output shaft','Output shaft','Output shaft',(#4246));
#4252=PRODUCT('Drive key','Drive key',$,(#4246));
#4253=PRODUCT('Drive pin','Drive pin','Drive pin',(#4246));
#4254=PRODUCT('Pivot bushing','Pivot bushing',$,(#4246));
#4255=PRODUCT('Wheel spacer','Wheel spacer',$,(#4246));
#4256=PRODUCT('Retaining spacer','Retaining spacer',$,(#4246));
#4257=PRODUCT('Pivot washer','Pivot washer',$,(#4246));
#4258=PRODUCT('Pivot retaining ring','Pivot retaining ring',$,(#4246));
#4259=PRESENTATION_STYLE_ASSIGNMENT((#4269));
#4260=PRESENTATION_STYLE_ASSIGNMENT((#4270));
#4261=PRESENTATION_STYLE_ASSIGNMENT((#4271));
#4262=PRESENTATION_STYLE_ASSIGNMENT((#4272));
#4263=PRESENTATION_STYLE_ASSIGNMENT((#4273));
#4264=PRESENTATION_STYLE_ASSIGNMENT((#4274));
#4265=PRESENTATION_STYLE_ASSIGNMENT((#4275));
#4266=PRESENTATION_STYLE_ASSIGNMENT((#4276));
#4267=PRESENTATION_STYLE_ASSIGNMENT((#4277));
#4268=PRESENTATION_STYLE_ASSIGNMENT((#4278));
#4269=SURFACE_STYLE_USAGE(.BOTH.,#4279);
#4270=SURFACE_STYLE_USAGE(.BOTH.,#4280);
#4271=SURFACE_STYLE_USAGE(.BOTH.,#4281);
#4272=SURFACE_STYLE_USAGE(.BOTH.,#4282);
#4273=SURFACE_STYLE_USAGE(.BOTH.,#4283);
#4274=SURFACE_STYLE_USAGE(.BOTH.,#4284);
#4275=SURFACE_STYLE_USAGE(.BOTH.,#4285);
#4276=SURFACE_STYLE_USAGE(.BOTH.,#4286);
#4277=SURFACE_STYLE_USAGE(.BOTH.,#4287);
#4278=SURFACE_STYLE_USAGE(.BOTH.,#4288);
#4279=SURFACE_SIDE_STYLE('',(#4289));
#4280=SURFACE_SIDE_STYLE('',(#4290));
#4281=SURFACE_SIDE_STYLE('',(#4291));
#4282=SURFACE_SIDE_STYLE('',(#4292));
#4283=SURFACE_SIDE_STYLE('',(#4293));
#4284=SURFACE_SIDE_STYLE('',(#4294));
#4285=SURFACE_SIDE_STYLE('',(#4295));
#4286=SURFACE_SIDE_STYLE('',(#4296));
#4287=SURFACE_SIDE_STYLE('',(#4297));
#4288=SURFACE_SIDE_STYLE('',(#4298));
#4289=SURFACE_STYLE_FILL_AREA(#4299);
#4290=SURFACE_STYLE_FILL_AREA(#4300);
#4291=SURFACE_STYLE_FILL_AREA(#4301);
#4292=SURFACE_STYLE_FILL_AREA(#4302);
#4293=SURFACE_STYLE_FILL_AREA(#4303);
#4294=SURFACE_STYLE_FILL_AREA(#4304);
#4295=SURFACE_STYLE_FILL_AREA(#4305);
#4296=SURFACE_STYLE_FILL_AREA(#4306);
#4297=SURFACE_STYLE_FILL_AREA(#4307);
#4298=SURFACE_STYLE_FILL_AREA(#4308);
#4299=FILL_AREA_STYLE('Steel - Satin',(#4309));
#4300=FILL_AREA_STYLE('Base gray',(#4310));
#4301=FILL_AREA_STYLE('Dark blue',(#4311));
#4302=FILL_AREA_STYLE('Sky blue',(#4312));
#4303=FILL_AREA_STYLE('Pivot gray',(#4313));
#4304=FILL_AREA_STYLE('Key gray',(#4314));
#4305=FILL_AREA_STYLE('Bearing light gray',(#4315));
#4306=FILL_AREA_STYLE('Spacer gray',(#4316));
#4307=FILL_AREA_STYLE('Washer light gray',(#4317));
#4308=FILL_AREA_STYLE('Dark gray',(#4318));
#4309=FILL_AREA_STYLE_COLOUR('Steel - Satin',#4319);
#4310=FILL_AREA_STYLE_COLOUR('Base gray',#4320);
#4311=FILL_AREA_STYLE_COLOUR('Dark blue',#4321);
#4312=FILL_AREA_STYLE_COLOUR('Sky blue',#4322);
#4313=FILL_AREA_STYLE_COLOUR('Pivot gray',#4323);
#4314=FILL_AREA_STYLE_COLOUR('Key gray',#4324);
#4315=FILL_AREA_STYLE_COLOUR('Bearing light gray',#4325);
#4316=FILL_AREA_STYLE_COLOUR('Spacer gray',#4326);
#4317=FILL_AREA_STYLE_COLOUR('Washer light gray',#4327);
#4318=FILL_AREA_STYLE_COLOUR('Dark gray',#4328);
#4319=COLOUR_RGB('Steel - Satin',0.627450980392157,0.627450980392157,0.627450980392157);
#4320=COLOUR_RGB('Base gray',0.407843137254902,0.447058823529412,0.498039215686275);
#4321=COLOUR_RGB('Dark blue',0.0901960784313725,0.270588235294118,0.513725490196078);
#4322=COLOUR_RGB('Sky blue',0.317647058823529,0.686274509803922,0.890196078431372);
#4323=COLOUR_RGB('Pivot gray',0.407843137254902,0.447058823529412,0.498039215686275);
#4324=COLOUR_RGB('Key gray',0.725490196078431,0.752941176470588,0.792156862745098);
#4325=COLOUR_RGB('Bearing light gray',0.725490196078431,0.752941176470588,
0.792156862745098);
#4326=COLOUR_RGB('Spacer gray',0.407843137254902,0.447058823529412,0.498039215686275);
#4327=COLOUR_RGB('Washer light gray',0.725490196078431,0.752941176470588,
0.792156862745098);
#4328=COLOUR_RGB('Dark gray',0.250980392156863,0.282352941176471,0.32156862745098);
ENDSEC;
END-ISO-10303-21;
